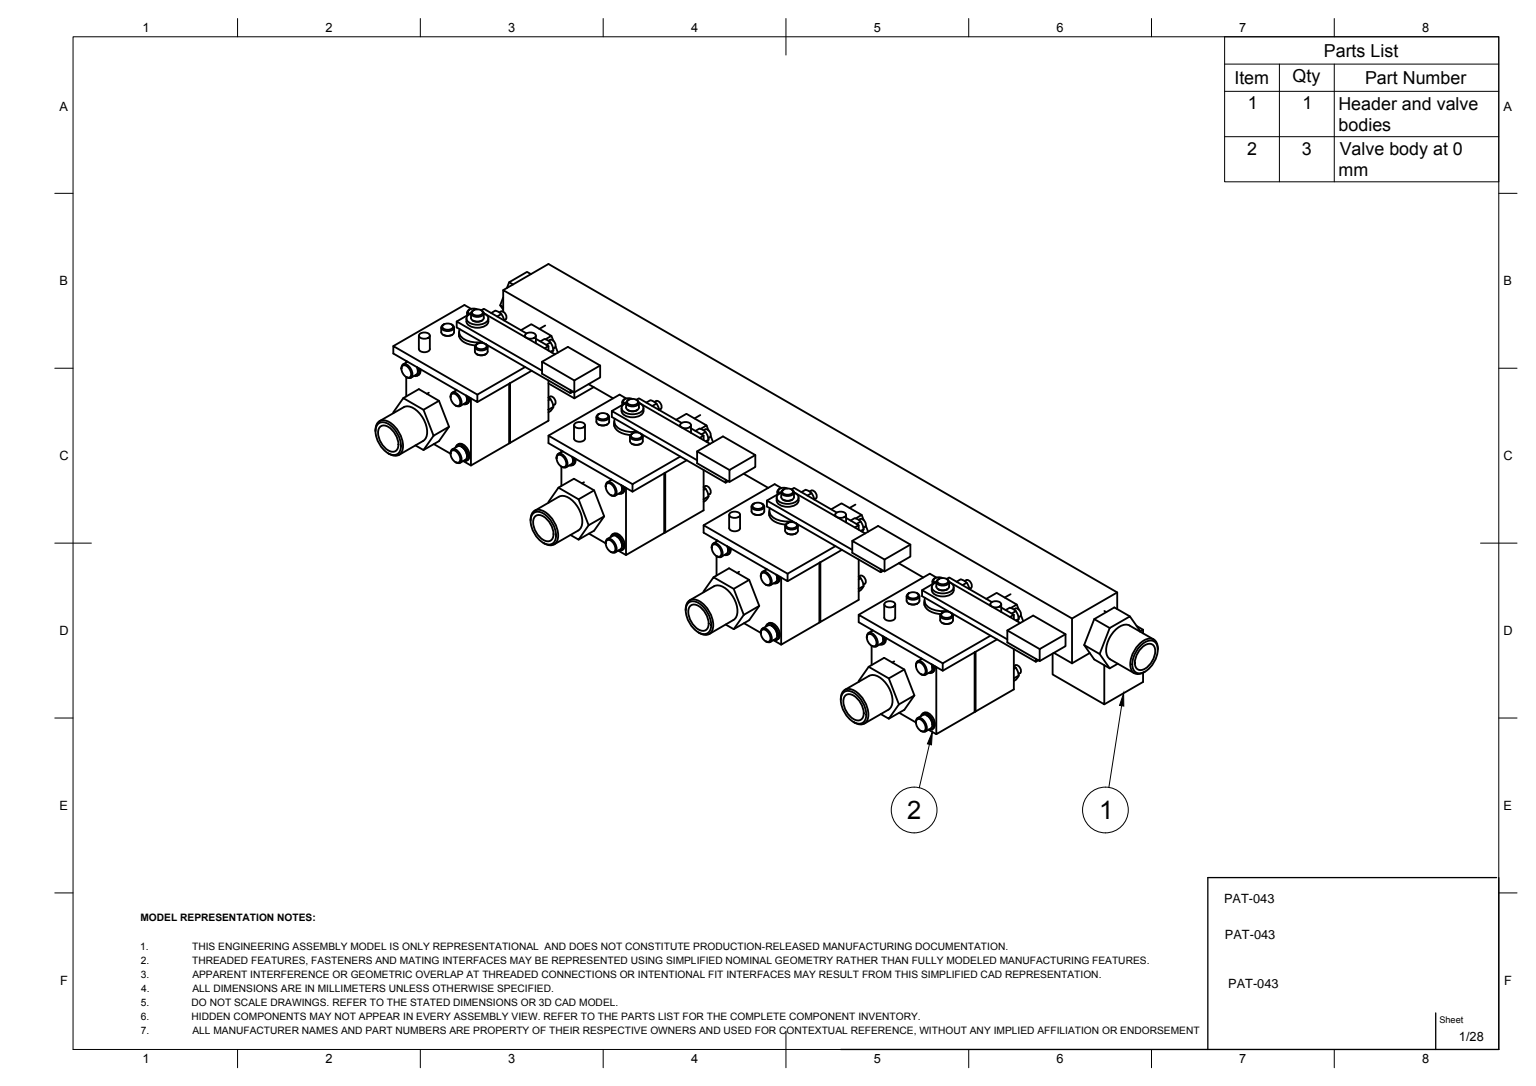
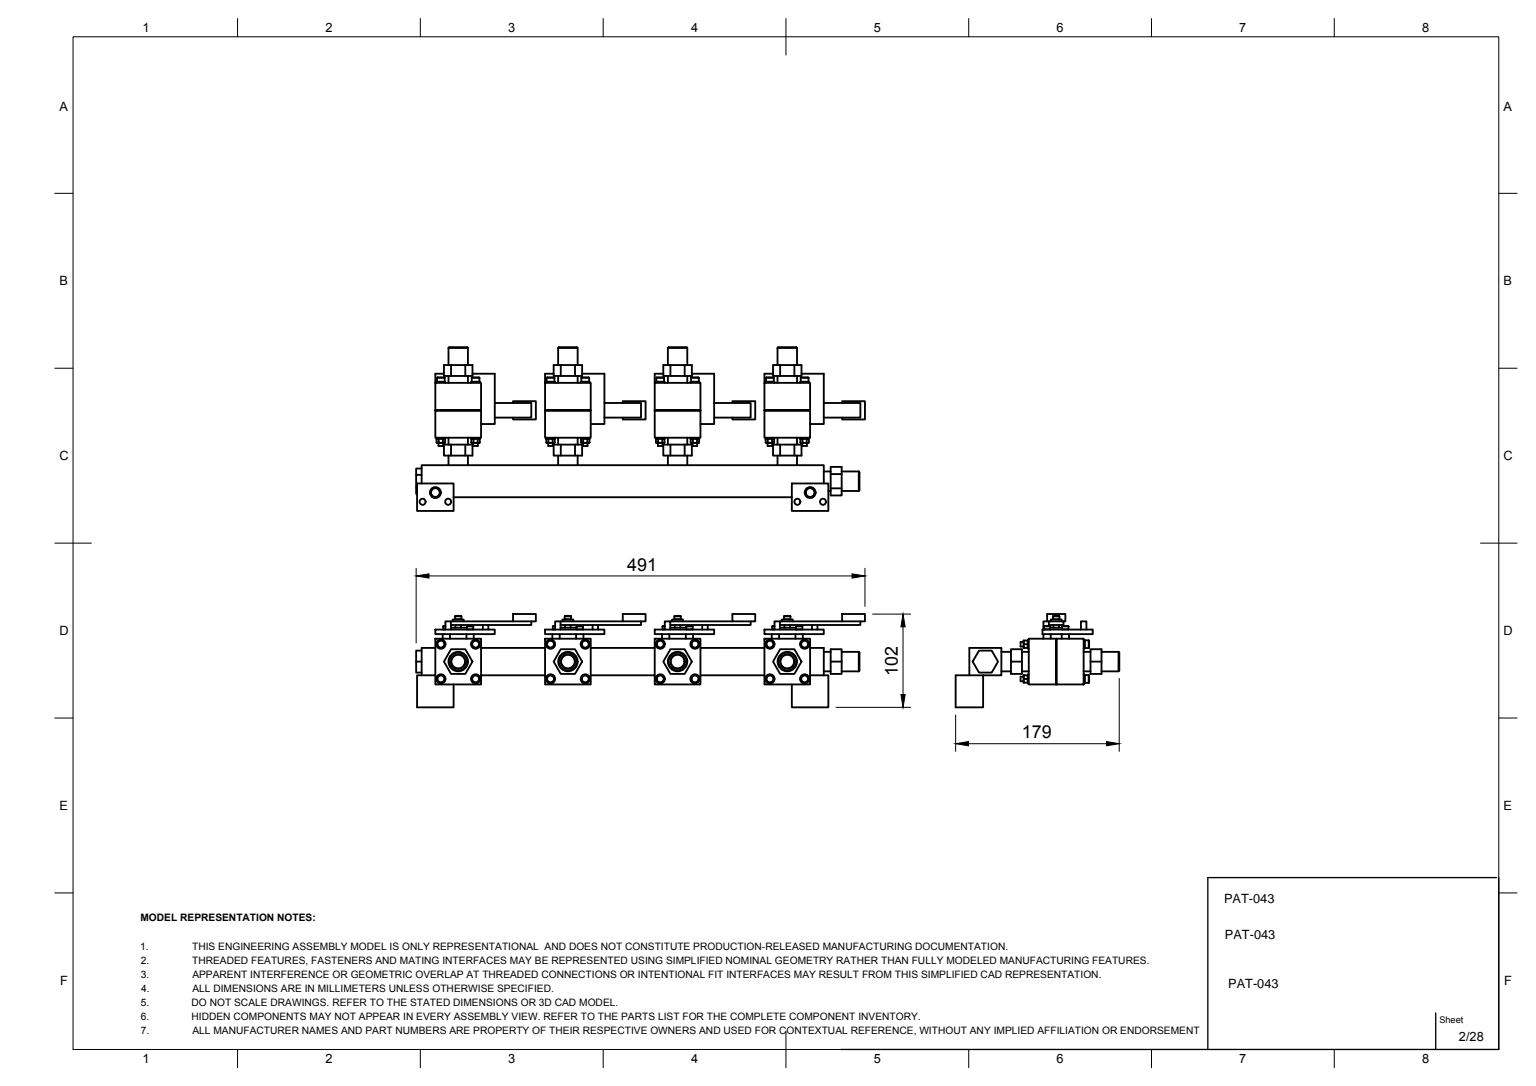
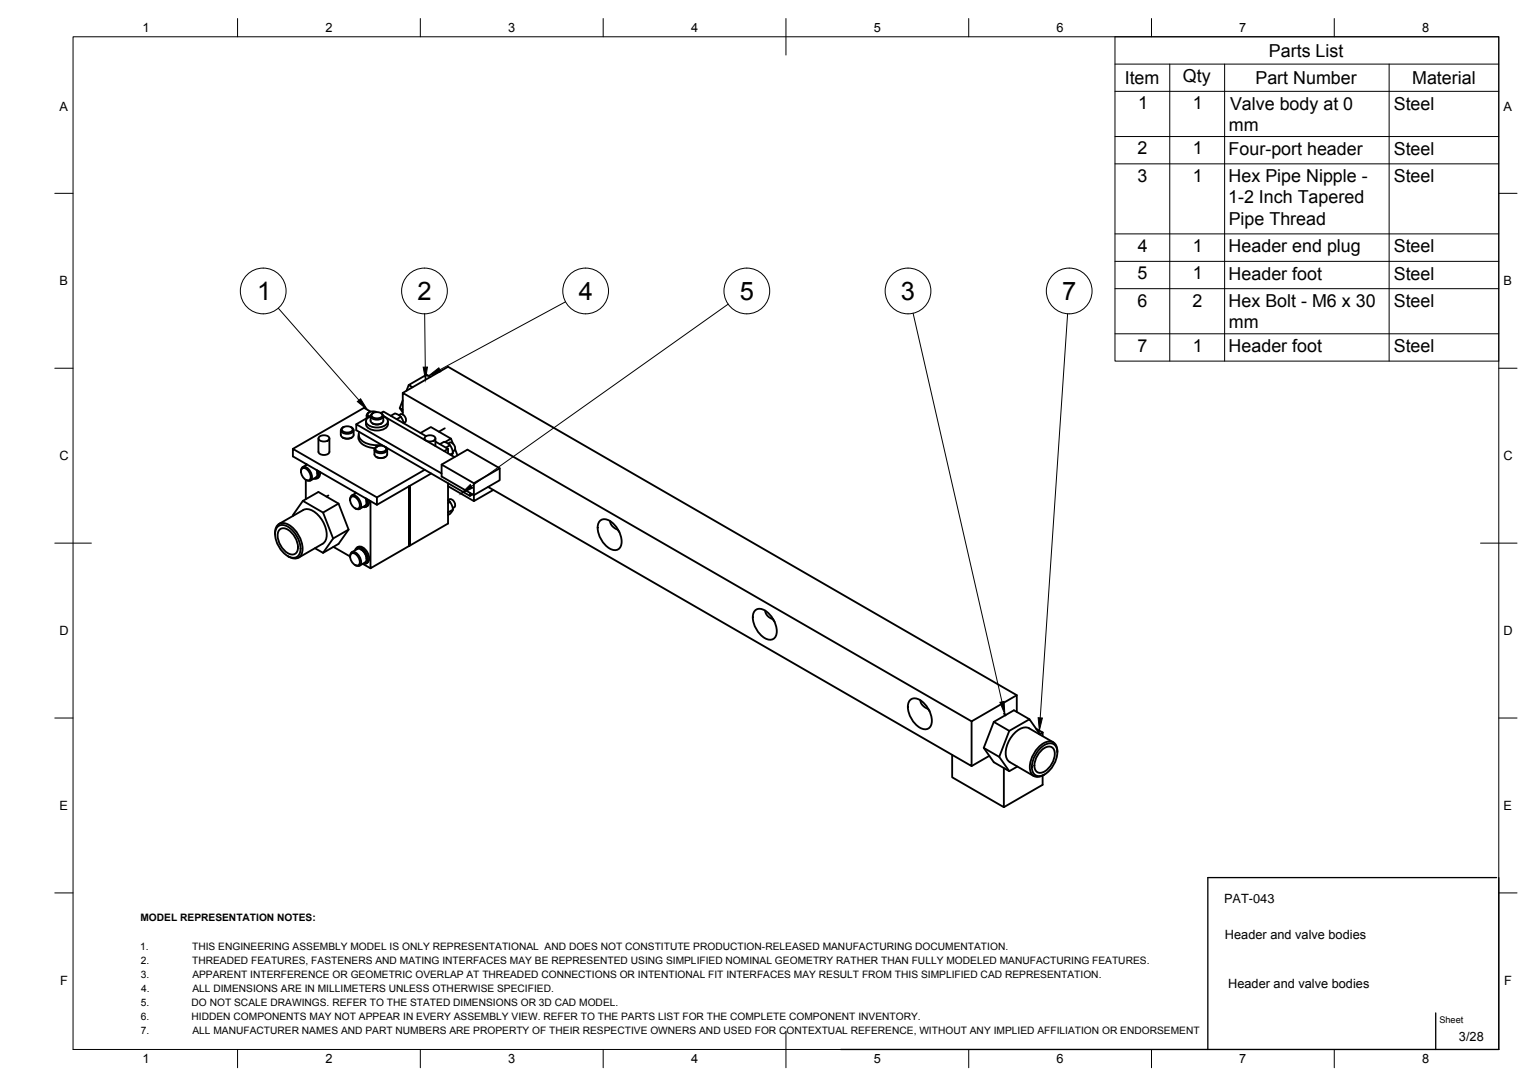
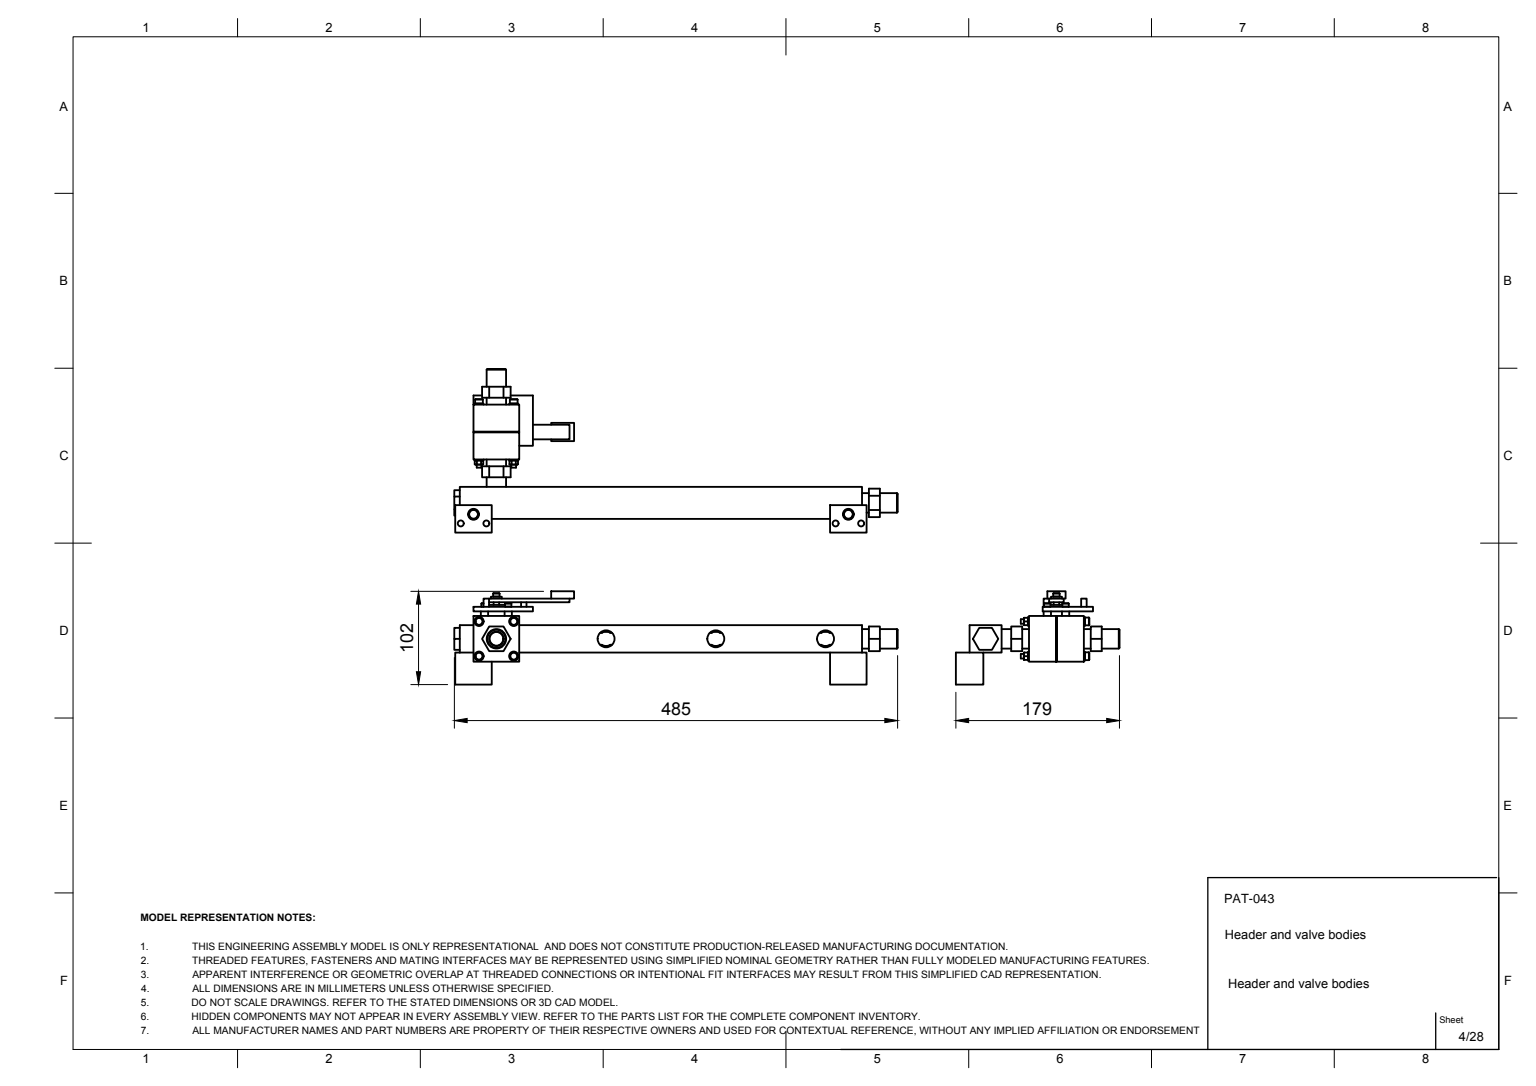
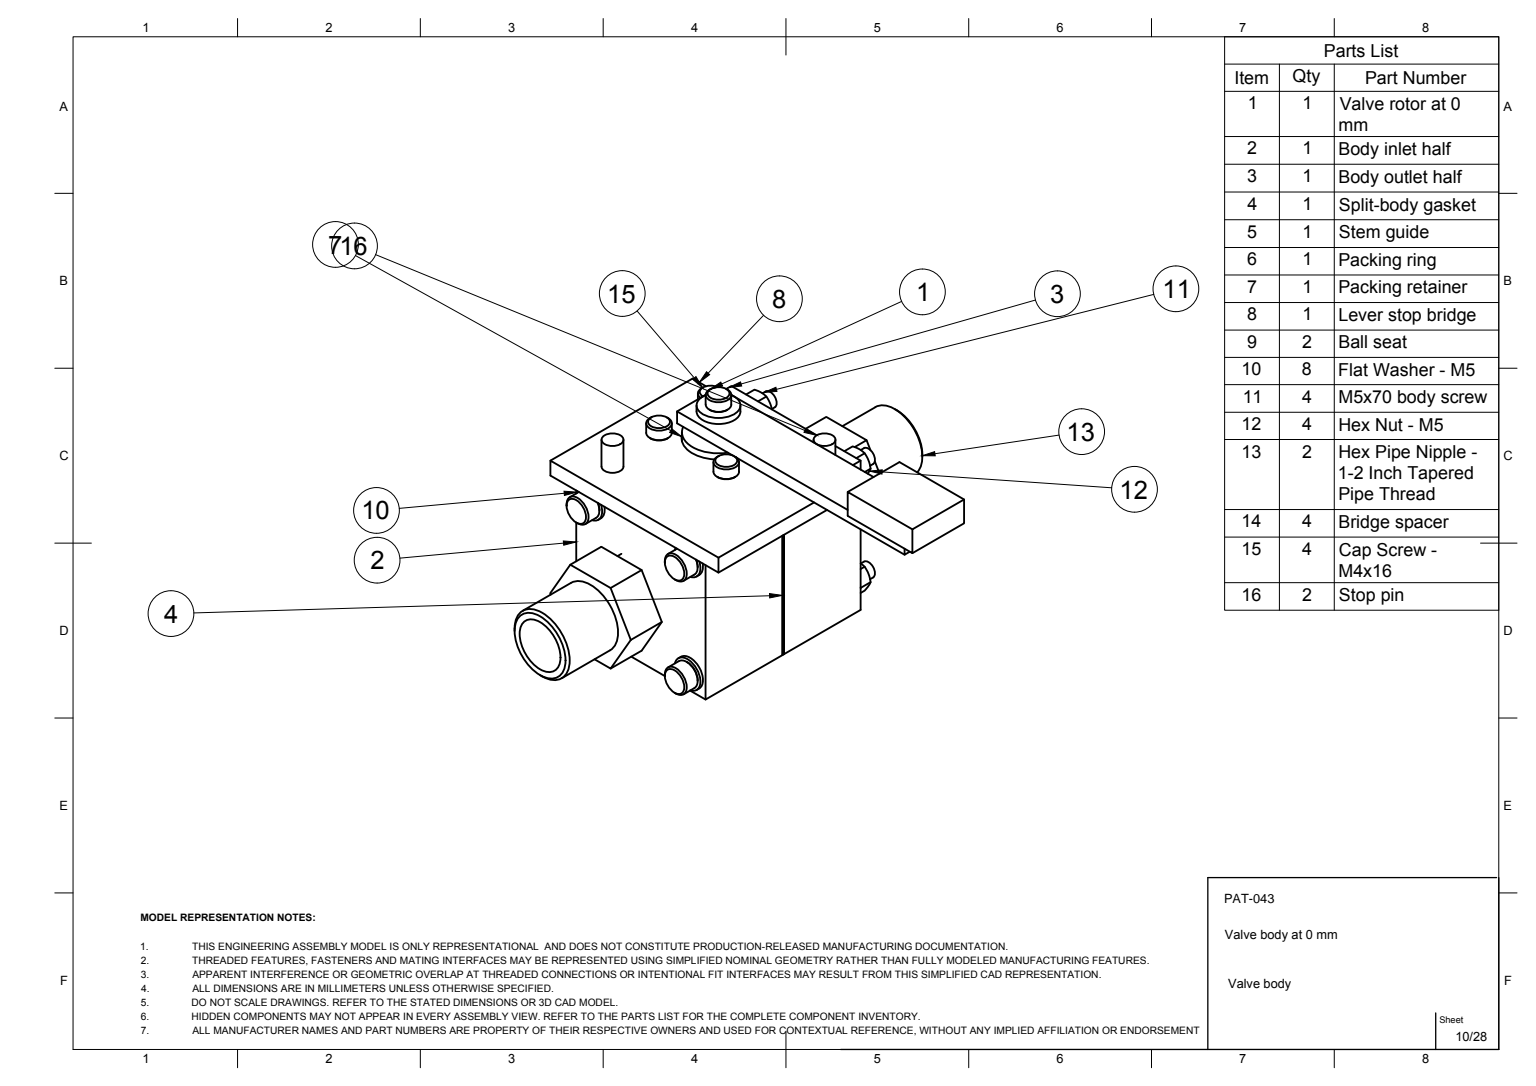
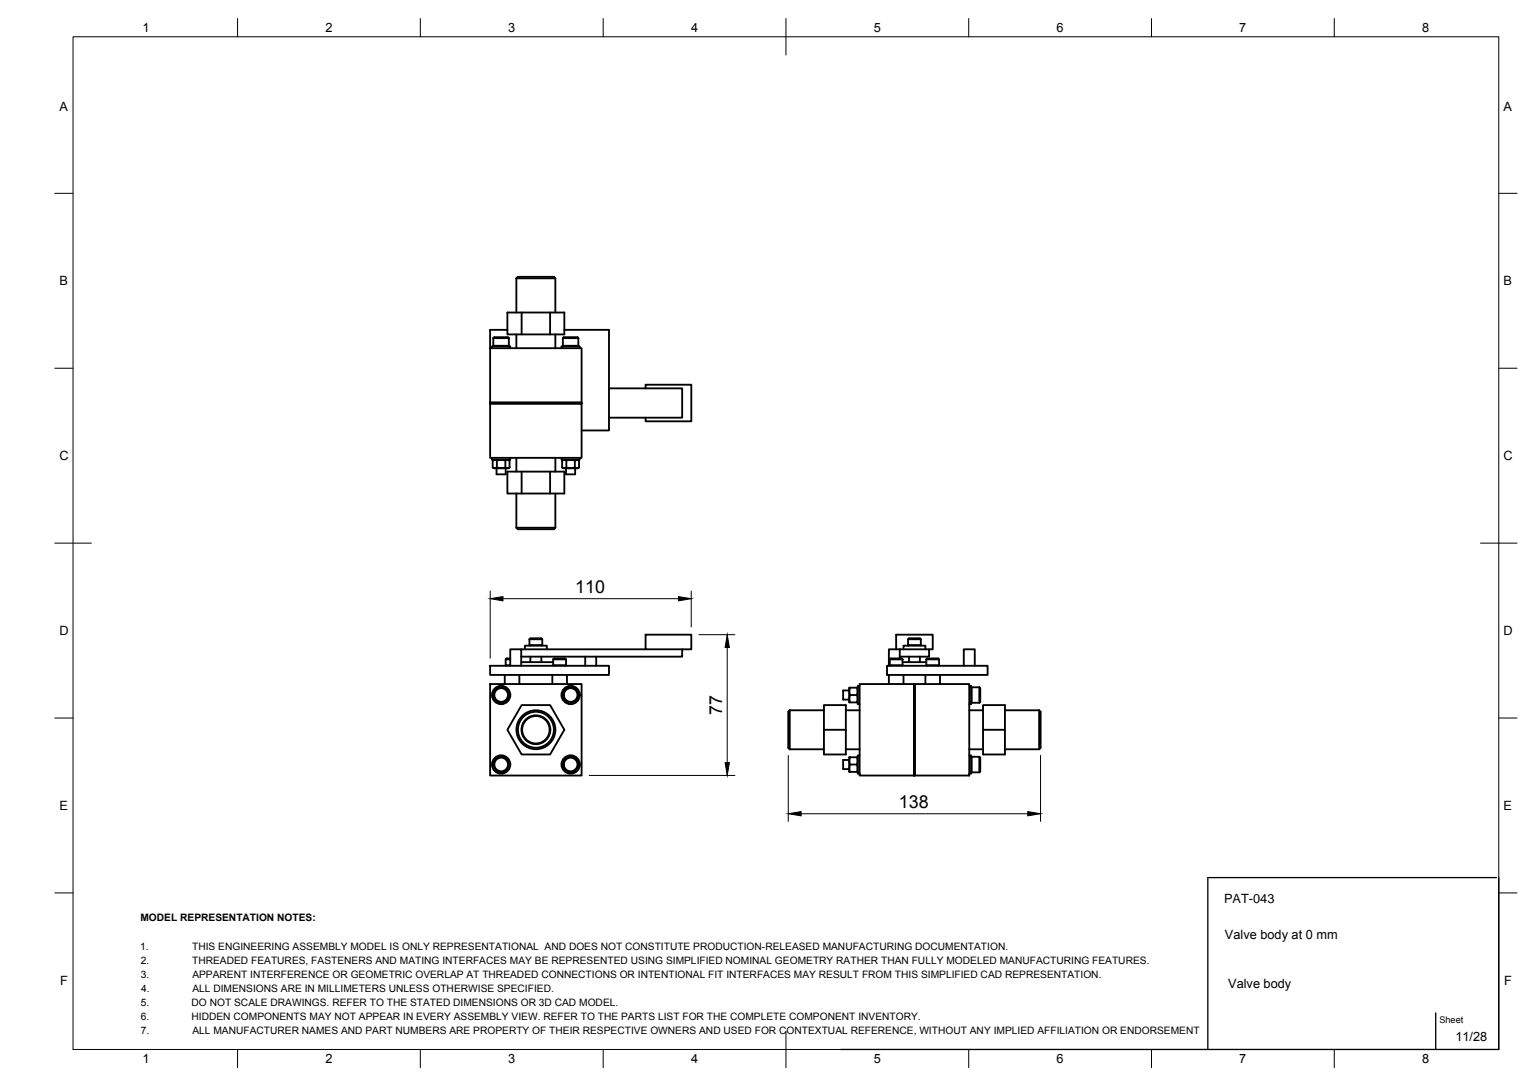
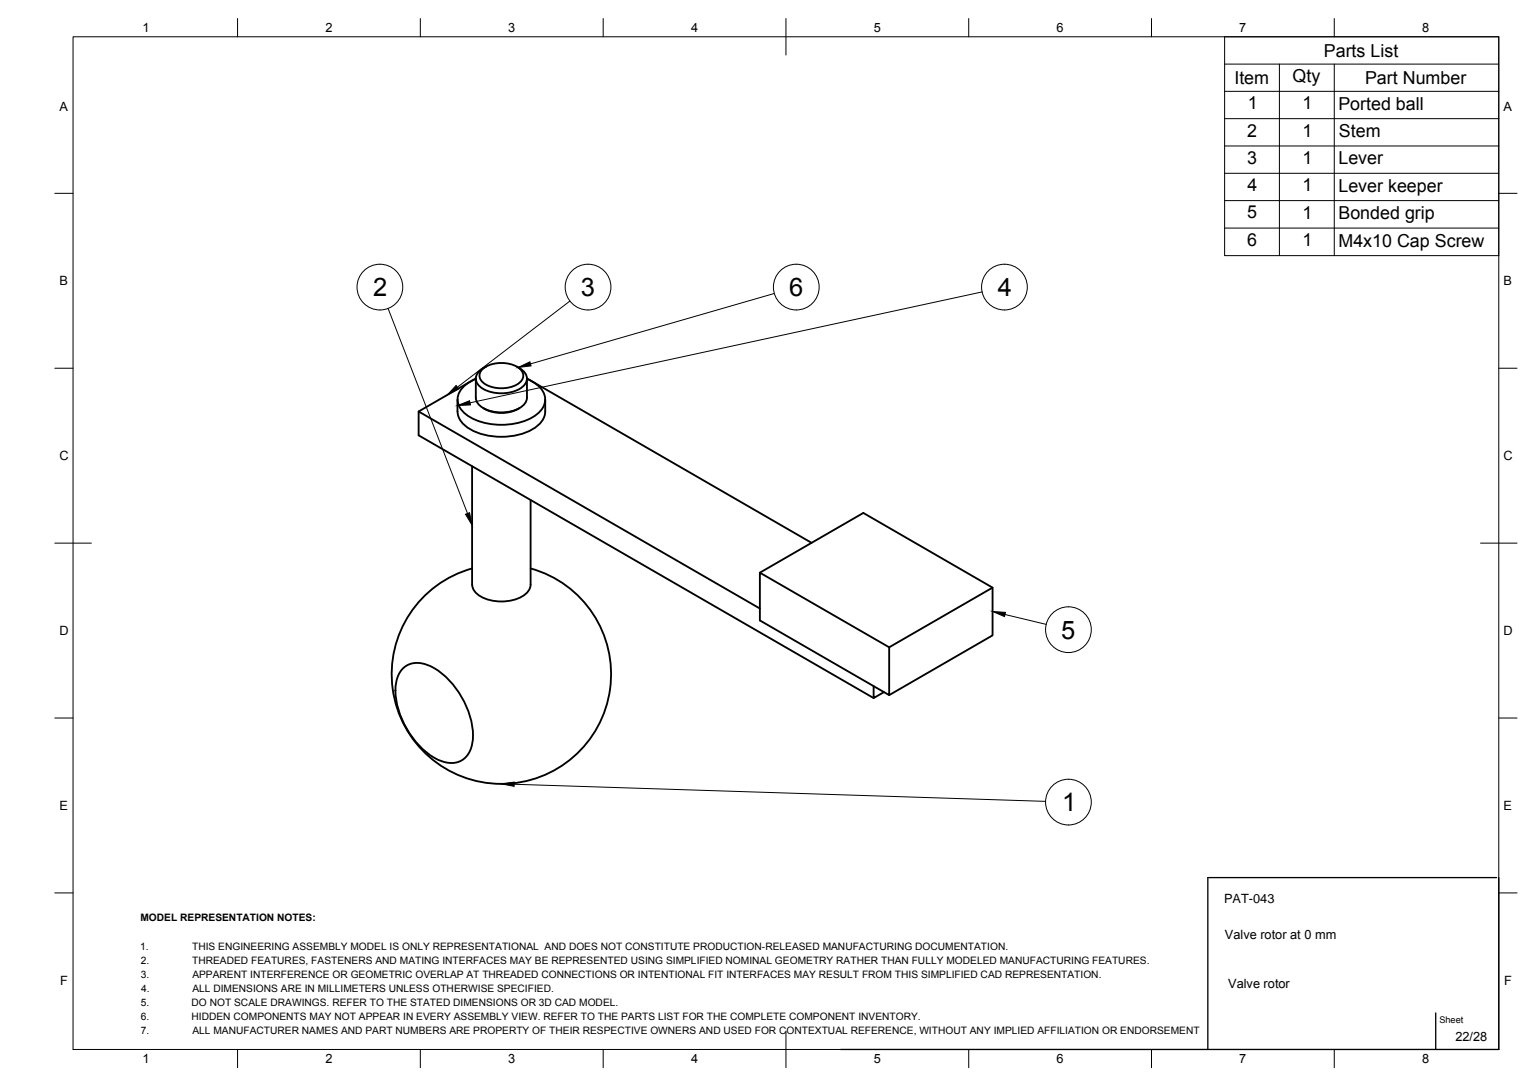
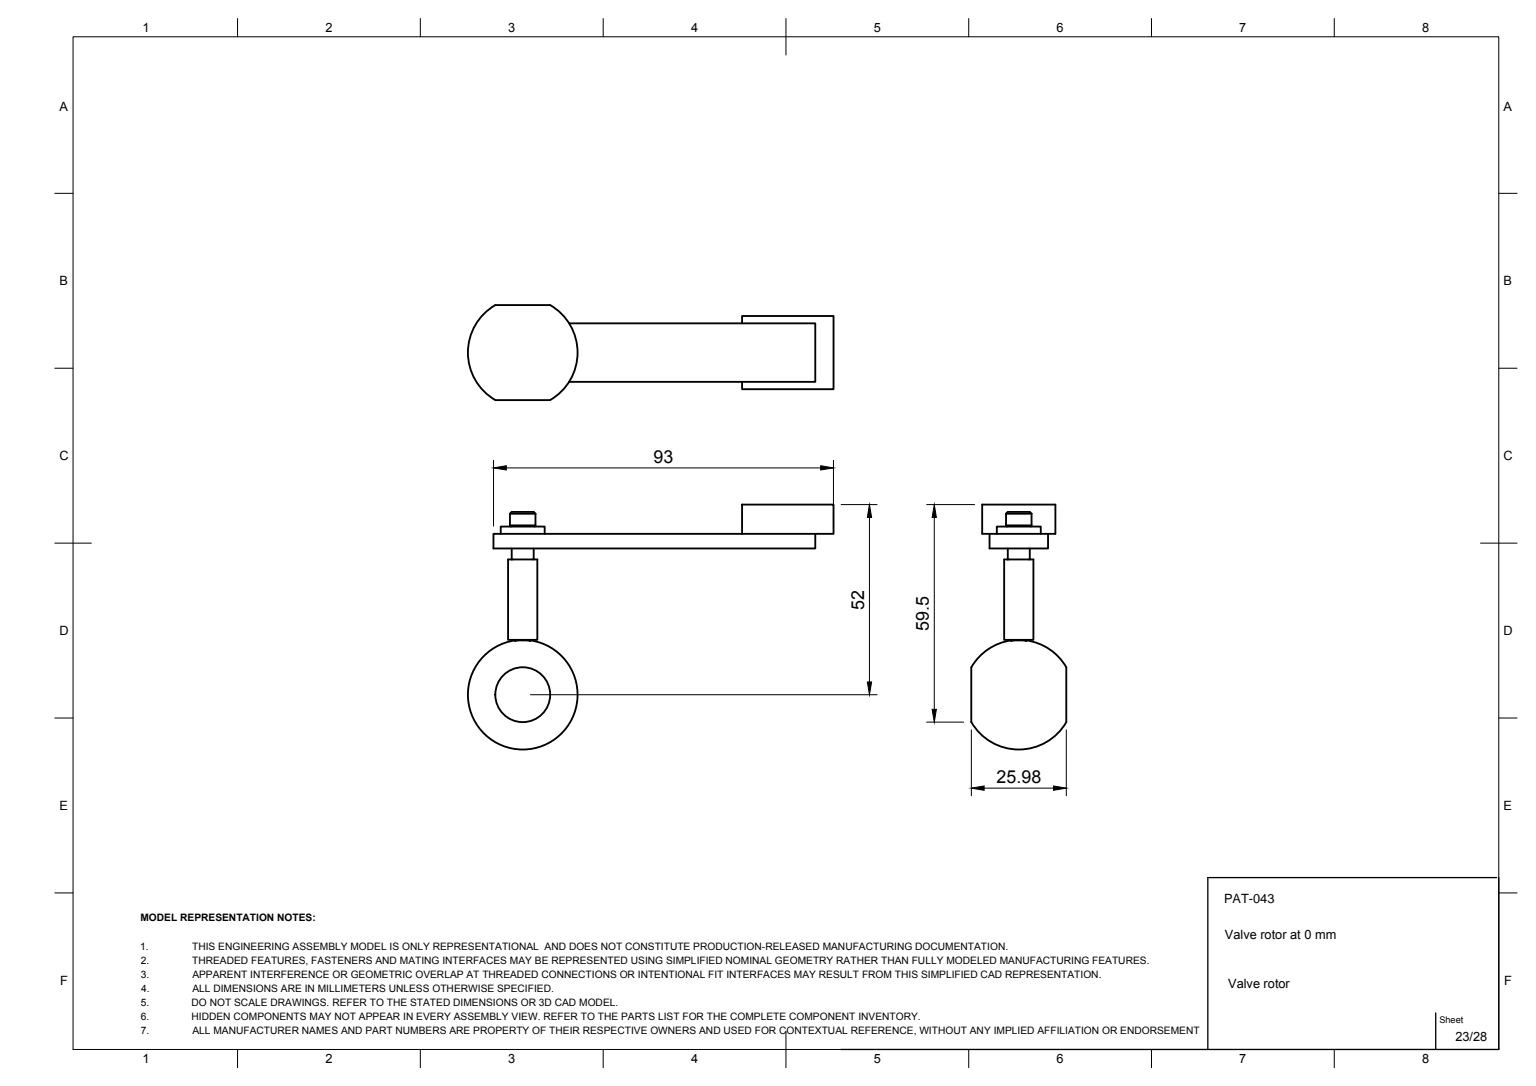
ISO-10303-21;
HEADER;
/* Generated by software containing ST-Developer
 * from STEP Tools, Inc. (www.steptools.com) 
 */

FILE_DESCRIPTION(
/* description */ ('Four-valve pipe header'),
/* implementation_level */ '2;1');

FILE_NAME(
/* name */ 'PAT-043',
/* time_stamp */ '2026-10-29T16:56:19-07:00',
/* author */ (''),
/* organization */ (''),
/* preprocessor_version */ 'ST-DEVELOPER v20.2',
/* originating_system */ 'Autodesk Translation Framework v15.17.0.0',
/* authorisation */ '');

FILE_SCHEMA (('AUTOMOTIVE_DESIGN { 1 0 10303 214 3 1 1 }'));
ENDSEC;

DATA;
#10=MECHANICAL_DESIGN_GEOMETRIC_PRESENTATION_REPRESENTATION('',(#333,#334,
#335,#336,#337,#338,#339,#340,#341,#342,#343,#344,#345,#346,#347,#348,#349,
#350,#351,#352,#353,#354,#355,#356,#357,#358),#10119);
#11=ITEM_DEFINED_TRANSFORMATION($,$,#6411,#6513);
#12=ITEM_DEFINED_TRANSFORMATION($,$,#6427,#6514);
#13=ITEM_DEFINED_TRANSFORMATION($,$,#6462,#6515);
#14=ITEM_DEFINED_TRANSFORMATION($,$,#6473,#6516);
#15=ITEM_DEFINED_TRANSFORMATION($,$,#6482,#6517);
#16=ITEM_DEFINED_TRANSFORMATION($,$,#6489,#6518);
#17=ITEM_DEFINED_TRANSFORMATION($,$,#6106,#6519);
#18=ITEM_DEFINED_TRANSFORMATION($,$,#6149,#6520);
#19=ITEM_DEFINED_TRANSFORMATION($,$,#6192,#6521);
#20=ITEM_DEFINED_TRANSFORMATION($,$,#6219,#6522);
#21=ITEM_DEFINED_TRANSFORMATION($,$,#6232,#6523);
#22=ITEM_DEFINED_TRANSFORMATION($,$,#6236,#6524);
#23=ITEM_DEFINED_TRANSFORMATION($,$,#6249,#6525);
#24=ITEM_DEFINED_TRANSFORMATION($,$,#6279,#6526);
#25=ITEM_DEFINED_TRANSFORMATION($,$,#6279,#6527);
#26=ITEM_DEFINED_TRANSFORMATION($,$,#6318,#6528);
#27=ITEM_DEFINED_TRANSFORMATION($,$,#6290,#6529);
#28=ITEM_DEFINED_TRANSFORMATION($,$,#6318,#6530);
#29=ITEM_DEFINED_TRANSFORMATION($,$,#6329,#6531);
#30=ITEM_DEFINED_TRANSFORMATION($,$,#6318,#6532);
#31=ITEM_DEFINED_TRANSFORMATION($,$,#6290,#6533);
#32=ITEM_DEFINED_TRANSFORMATION($,$,#6318,#6534);
#33=ITEM_DEFINED_TRANSFORMATION($,$,#6329,#6535);
#34=ITEM_DEFINED_TRANSFORMATION($,$,#6318,#6536);
#35=ITEM_DEFINED_TRANSFORMATION($,$,#6290,#6537);
#36=ITEM_DEFINED_TRANSFORMATION($,$,#6318,#6538);
#37=ITEM_DEFINED_TRANSFORMATION($,$,#6329,#6539);
#38=ITEM_DEFINED_TRANSFORMATION($,$,#6318,#6540);
#39=ITEM_DEFINED_TRANSFORMATION($,$,#6290,#6541);
#40=ITEM_DEFINED_TRANSFORMATION($,$,#6318,#6542);
#41=ITEM_DEFINED_TRANSFORMATION($,$,#6329,#6543);
#42=ITEM_DEFINED_TRANSFORMATION($,$,#6345,#6544);
#43=ITEM_DEFINED_TRANSFORMATION($,$,#6345,#6545);
#44=ITEM_DEFINED_TRANSFORMATION($,$,#6369,#6546);
#45=ITEM_DEFINED_TRANSFORMATION($,$,#6378,#6547);
#46=ITEM_DEFINED_TRANSFORMATION($,$,#6369,#6548);
#47=ITEM_DEFINED_TRANSFORMATION($,$,#6378,#6549);
#48=ITEM_DEFINED_TRANSFORMATION($,$,#6369,#6550);
#49=ITEM_DEFINED_TRANSFORMATION($,$,#6378,#6551);
#50=ITEM_DEFINED_TRANSFORMATION($,$,#6369,#6552);
#51=ITEM_DEFINED_TRANSFORMATION($,$,#6378,#6553);
#52=ITEM_DEFINED_TRANSFORMATION($,$,#6404,#6554);
#53=ITEM_DEFINED_TRANSFORMATION($,$,#6404,#6555);
#54=ITEM_DEFINED_TRANSFORMATION($,$,#6410,#6556);
#55=ITEM_DEFINED_TRANSFORMATION($,$,#6105,#6557);
#56=ITEM_DEFINED_TRANSFORMATION($,$,#5897,#6558);
#57=ITEM_DEFINED_TRANSFORMATION($,$,#6019,#6559);
#58=ITEM_DEFINED_TRANSFORMATION($,$,#6032,#6560);
#59=ITEM_DEFINED_TRANSFORMATION($,$,#6060,#6561);
#60=ITEM_DEFINED_TRANSFORMATION($,$,#6345,#6562);
#61=ITEM_DEFINED_TRANSFORMATION($,$,#6088,#6563);
#62=ITEM_DEFINED_TRANSFORMATION($,$,#6088,#6564);
#63=ITEM_DEFINED_TRANSFORMATION($,$,#5896,#6565);
#64=ITEM_DEFINED_TRANSFORMATION($,$,#6105,#6566);
#65=ITEM_DEFINED_TRANSFORMATION($,$,#6105,#6567);
#66=ITEM_DEFINED_TRANSFORMATION($,$,#6105,#6568);
#67=(
REPRESENTATION_RELATIONSHIP($,$,#10264,#10263)
REPRESENTATION_RELATIONSHIP_WITH_TRANSFORMATION(#11)
SHAPE_REPRESENTATION_RELATIONSHIP()
);
#68=(
REPRESENTATION_RELATIONSHIP($,$,#10265,#10263)
REPRESENTATION_RELATIONSHIP_WITH_TRANSFORMATION(#12)
SHAPE_REPRESENTATION_RELATIONSHIP()
);
#69=(
REPRESENTATION_RELATIONSHIP($,$,#10266,#10263)
REPRESENTATION_RELATIONSHIP_WITH_TRANSFORMATION(#13)
SHAPE_REPRESENTATION_RELATIONSHIP()
);
#70=(
REPRESENTATION_RELATIONSHIP($,$,#10267,#10263)
REPRESENTATION_RELATIONSHIP_WITH_TRANSFORMATION(#14)
SHAPE_REPRESENTATION_RELATIONSHIP()
);
#71=(
REPRESENTATION_RELATIONSHIP($,$,#10268,#10263)
REPRESENTATION_RELATIONSHIP_WITH_TRANSFORMATION(#15)
SHAPE_REPRESENTATION_RELATIONSHIP()
);
#72=(
REPRESENTATION_RELATIONSHIP($,$,#10269,#10263)
REPRESENTATION_RELATIONSHIP_WITH_TRANSFORMATION(#16)
SHAPE_REPRESENTATION_RELATIONSHIP()
);
#73=(
REPRESENTATION_RELATIONSHIP($,$,#10248,#10247)
REPRESENTATION_RELATIONSHIP_WITH_TRANSFORMATION(#17)
SHAPE_REPRESENTATION_RELATIONSHIP()
);
#74=(
REPRESENTATION_RELATIONSHIP($,$,#10249,#10247)
REPRESENTATION_RELATIONSHIP_WITH_TRANSFORMATION(#18)
SHAPE_REPRESENTATION_RELATIONSHIP()
);
#75=(
REPRESENTATION_RELATIONSHIP($,$,#10250,#10247)
REPRESENTATION_RELATIONSHIP_WITH_TRANSFORMATION(#19)
SHAPE_REPRESENTATION_RELATIONSHIP()
);
#76=(
REPRESENTATION_RELATIONSHIP($,$,#10251,#10247)
REPRESENTATION_RELATIONSHIP_WITH_TRANSFORMATION(#20)
SHAPE_REPRESENTATION_RELATIONSHIP()
);
#77=(
REPRESENTATION_RELATIONSHIP($,$,#10252,#10247)
REPRESENTATION_RELATIONSHIP_WITH_TRANSFORMATION(#21)
SHAPE_REPRESENTATION_RELATIONSHIP()
);
#78=(
REPRESENTATION_RELATIONSHIP($,$,#10253,#10247)
REPRESENTATION_RELATIONSHIP_WITH_TRANSFORMATION(#22)
SHAPE_REPRESENTATION_RELATIONSHIP()
);
#79=(
REPRESENTATION_RELATIONSHIP($,$,#10254,#10247)
REPRESENTATION_RELATIONSHIP_WITH_TRANSFORMATION(#23)
SHAPE_REPRESENTATION_RELATIONSHIP()
);
#80=(
REPRESENTATION_RELATIONSHIP($,$,#10255,#10247)
REPRESENTATION_RELATIONSHIP_WITH_TRANSFORMATION(#24)
SHAPE_REPRESENTATION_RELATIONSHIP()
);
#81=(
REPRESENTATION_RELATIONSHIP($,$,#10255,#10247)
REPRESENTATION_RELATIONSHIP_WITH_TRANSFORMATION(#25)
SHAPE_REPRESENTATION_RELATIONSHIP()
);
#82=(
REPRESENTATION_RELATIONSHIP($,$,#10257,#10247)
REPRESENTATION_RELATIONSHIP_WITH_TRANSFORMATION(#26)
SHAPE_REPRESENTATION_RELATIONSHIP()
);
#83=(
REPRESENTATION_RELATIONSHIP($,$,#10256,#10247)
REPRESENTATION_RELATIONSHIP_WITH_TRANSFORMATION(#27)
SHAPE_REPRESENTATION_RELATIONSHIP()
);
#84=(
REPRESENTATION_RELATIONSHIP($,$,#10257,#10247)
REPRESENTATION_RELATIONSHIP_WITH_TRANSFORMATION(#28)
SHAPE_REPRESENTATION_RELATIONSHIP()
);
#85=(
REPRESENTATION_RELATIONSHIP($,$,#10258,#10247)
REPRESENTATION_RELATIONSHIP_WITH_TRANSFORMATION(#29)
SHAPE_REPRESENTATION_RELATIONSHIP()
);
#86=(
REPRESENTATION_RELATIONSHIP($,$,#10257,#10247)
REPRESENTATION_RELATIONSHIP_WITH_TRANSFORMATION(#30)
SHAPE_REPRESENTATION_RELATIONSHIP()
);
#87=(
REPRESENTATION_RELATIONSHIP($,$,#10256,#10247)
REPRESENTATION_RELATIONSHIP_WITH_TRANSFORMATION(#31)
SHAPE_REPRESENTATION_RELATIONSHIP()
);
#88=(
REPRESENTATION_RELATIONSHIP($,$,#10257,#10247)
REPRESENTATION_RELATIONSHIP_WITH_TRANSFORMATION(#32)
SHAPE_REPRESENTATION_RELATIONSHIP()
);
#89=(
REPRESENTATION_RELATIONSHIP($,$,#10258,#10247)
REPRESENTATION_RELATIONSHIP_WITH_TRANSFORMATION(#33)
SHAPE_REPRESENTATION_RELATIONSHIP()
);
#90=(
REPRESENTATION_RELATIONSHIP($,$,#10257,#10247)
REPRESENTATION_RELATIONSHIP_WITH_TRANSFORMATION(#34)
SHAPE_REPRESENTATION_RELATIONSHIP()
);
#91=(
REPRESENTATION_RELATIONSHIP($,$,#10256,#10247)
REPRESENTATION_RELATIONSHIP_WITH_TRANSFORMATION(#35)
SHAPE_REPRESENTATION_RELATIONSHIP()
);
#92=(
REPRESENTATION_RELATIONSHIP($,$,#10257,#10247)
REPRESENTATION_RELATIONSHIP_WITH_TRANSFORMATION(#36)
SHAPE_REPRESENTATION_RELATIONSHIP()
);
#93=(
REPRESENTATION_RELATIONSHIP($,$,#10258,#10247)
REPRESENTATION_RELATIONSHIP_WITH_TRANSFORMATION(#37)
SHAPE_REPRESENTATION_RELATIONSHIP()
);
#94=(
REPRESENTATION_RELATIONSHIP($,$,#10257,#10247)
REPRESENTATION_RELATIONSHIP_WITH_TRANSFORMATION(#38)
SHAPE_REPRESENTATION_RELATIONSHIP()
);
#95=(
REPRESENTATION_RELATIONSHIP($,$,#10256,#10247)
REPRESENTATION_RELATIONSHIP_WITH_TRANSFORMATION(#39)
SHAPE_REPRESENTATION_RELATIONSHIP()
);
#96=(
REPRESENTATION_RELATIONSHIP($,$,#10257,#10247)
REPRESENTATION_RELATIONSHIP_WITH_TRANSFORMATION(#40)
SHAPE_REPRESENTATION_RELATIONSHIP()
);
#97=(
REPRESENTATION_RELATIONSHIP($,$,#10258,#10247)
REPRESENTATION_RELATIONSHIP_WITH_TRANSFORMATION(#41)
SHAPE_REPRESENTATION_RELATIONSHIP()
);
#98=(
REPRESENTATION_RELATIONSHIP($,$,#10259,#10247)
REPRESENTATION_RELATIONSHIP_WITH_TRANSFORMATION(#42)
SHAPE_REPRESENTATION_RELATIONSHIP()
);
#99=(
REPRESENTATION_RELATIONSHIP($,$,#10259,#10247)
REPRESENTATION_RELATIONSHIP_WITH_TRANSFORMATION(#43)
SHAPE_REPRESENTATION_RELATIONSHIP()
);
#100=(
REPRESENTATION_RELATIONSHIP($,$,#10260,#10247)
REPRESENTATION_RELATIONSHIP_WITH_TRANSFORMATION(#44)
SHAPE_REPRESENTATION_RELATIONSHIP()
);
#101=(
REPRESENTATION_RELATIONSHIP($,$,#10261,#10247)
REPRESENTATION_RELATIONSHIP_WITH_TRANSFORMATION(#45)
SHAPE_REPRESENTATION_RELATIONSHIP()
);
#102=(
REPRESENTATION_RELATIONSHIP($,$,#10260,#10247)
REPRESENTATION_RELATIONSHIP_WITH_TRANSFORMATION(#46)
SHAPE_REPRESENTATION_RELATIONSHIP()
);
#103=(
REPRESENTATION_RELATIONSHIP($,$,#10261,#10247)
REPRESENTATION_RELATIONSHIP_WITH_TRANSFORMATION(#47)
SHAPE_REPRESENTATION_RELATIONSHIP()
);
#104=(
REPRESENTATION_RELATIONSHIP($,$,#10260,#10247)
REPRESENTATION_RELATIONSHIP_WITH_TRANSFORMATION(#48)
SHAPE_REPRESENTATION_RELATIONSHIP()
);
#105=(
REPRESENTATION_RELATIONSHIP($,$,#10261,#10247)
REPRESENTATION_RELATIONSHIP_WITH_TRANSFORMATION(#49)
SHAPE_REPRESENTATION_RELATIONSHIP()
);
#106=(
REPRESENTATION_RELATIONSHIP($,$,#10260,#10247)
REPRESENTATION_RELATIONSHIP_WITH_TRANSFORMATION(#50)
SHAPE_REPRESENTATION_RELATIONSHIP()
);
#107=(
REPRESENTATION_RELATIONSHIP($,$,#10261,#10247)
REPRESENTATION_RELATIONSHIP_WITH_TRANSFORMATION(#51)
SHAPE_REPRESENTATION_RELATIONSHIP()
);
#108=(
REPRESENTATION_RELATIONSHIP($,$,#10262,#10247)
REPRESENTATION_RELATIONSHIP_WITH_TRANSFORMATION(#52)
SHAPE_REPRESENTATION_RELATIONSHIP()
);
#109=(
REPRESENTATION_RELATIONSHIP($,$,#10262,#10247)
REPRESENTATION_RELATIONSHIP_WITH_TRANSFORMATION(#53)
SHAPE_REPRESENTATION_RELATIONSHIP()
);
#110=(
REPRESENTATION_RELATIONSHIP($,$,#10263,#10247)
REPRESENTATION_RELATIONSHIP_WITH_TRANSFORMATION(#54)
SHAPE_REPRESENTATION_RELATIONSHIP()
);
#111=(
REPRESENTATION_RELATIONSHIP($,$,#10247,#10241)
REPRESENTATION_RELATIONSHIP_WITH_TRANSFORMATION(#55)
SHAPE_REPRESENTATION_RELATIONSHIP()
);
#112=(
REPRESENTATION_RELATIONSHIP($,$,#10242,#10241)
REPRESENTATION_RELATIONSHIP_WITH_TRANSFORMATION(#56)
SHAPE_REPRESENTATION_RELATIONSHIP()
);
#113=(
REPRESENTATION_RELATIONSHIP($,$,#10243,#10241)
REPRESENTATION_RELATIONSHIP_WITH_TRANSFORMATION(#57)
SHAPE_REPRESENTATION_RELATIONSHIP()
);
#114=(
REPRESENTATION_RELATIONSHIP($,$,#10244,#10241)
REPRESENTATION_RELATIONSHIP_WITH_TRANSFORMATION(#58)
SHAPE_REPRESENTATION_RELATIONSHIP()
);
#115=(
REPRESENTATION_RELATIONSHIP($,$,#10245,#10241)
REPRESENTATION_RELATIONSHIP_WITH_TRANSFORMATION(#59)
SHAPE_REPRESENTATION_RELATIONSHIP()
);
#116=(
REPRESENTATION_RELATIONSHIP($,$,#10259,#10241)
REPRESENTATION_RELATIONSHIP_WITH_TRANSFORMATION(#60)
SHAPE_REPRESENTATION_RELATIONSHIP()
);
#117=(
REPRESENTATION_RELATIONSHIP($,$,#10246,#10241)
REPRESENTATION_RELATIONSHIP_WITH_TRANSFORMATION(#61)
SHAPE_REPRESENTATION_RELATIONSHIP()
);
#118=(
REPRESENTATION_RELATIONSHIP($,$,#10246,#10241)
REPRESENTATION_RELATIONSHIP_WITH_TRANSFORMATION(#62)
SHAPE_REPRESENTATION_RELATIONSHIP()
);
#119=(
REPRESENTATION_RELATIONSHIP($,$,#10241,#10240)
REPRESENTATION_RELATIONSHIP_WITH_TRANSFORMATION(#63)
SHAPE_REPRESENTATION_RELATIONSHIP()
);
#120=(
REPRESENTATION_RELATIONSHIP($,$,#10247,#10240)
REPRESENTATION_RELATIONSHIP_WITH_TRANSFORMATION(#64)
SHAPE_REPRESENTATION_RELATIONSHIP()
);
#121=(
REPRESENTATION_RELATIONSHIP($,$,#10247,#10240)
REPRESENTATION_RELATIONSHIP_WITH_TRANSFORMATION(#65)
SHAPE_REPRESENTATION_RELATIONSHIP()
);
#122=(
REPRESENTATION_RELATIONSHIP($,$,#10247,#10240)
REPRESENTATION_RELATIONSHIP_WITH_TRANSFORMATION(#66)
SHAPE_REPRESENTATION_RELATIONSHIP()
);
#123=CONTEXT_DEPENDENT_SHAPE_REPRESENTATION(#67,#10184);
#124=CONTEXT_DEPENDENT_SHAPE_REPRESENTATION(#68,#10185);
#125=CONTEXT_DEPENDENT_SHAPE_REPRESENTATION(#69,#10186);
#126=CONTEXT_DEPENDENT_SHAPE_REPRESENTATION(#70,#10187);
#127=CONTEXT_DEPENDENT_SHAPE_REPRESENTATION(#71,#10188);
#128=CONTEXT_DEPENDENT_SHAPE_REPRESENTATION(#72,#10189);
#129=CONTEXT_DEPENDENT_SHAPE_REPRESENTATION(#73,#10190);
#130=CONTEXT_DEPENDENT_SHAPE_REPRESENTATION(#74,#10191);
#131=CONTEXT_DEPENDENT_SHAPE_REPRESENTATION(#75,#10192);
#132=CONTEXT_DEPENDENT_SHAPE_REPRESENTATION(#76,#10193);
#133=CONTEXT_DEPENDENT_SHAPE_REPRESENTATION(#77,#10194);
#134=CONTEXT_DEPENDENT_SHAPE_REPRESENTATION(#78,#10195);
#135=CONTEXT_DEPENDENT_SHAPE_REPRESENTATION(#79,#10196);
#136=CONTEXT_DEPENDENT_SHAPE_REPRESENTATION(#80,#10197);
#137=CONTEXT_DEPENDENT_SHAPE_REPRESENTATION(#81,#10198);
#138=CONTEXT_DEPENDENT_SHAPE_REPRESENTATION(#82,#10199);
#139=CONTEXT_DEPENDENT_SHAPE_REPRESENTATION(#83,#10200);
#140=CONTEXT_DEPENDENT_SHAPE_REPRESENTATION(#84,#10201);
#141=CONTEXT_DEPENDENT_SHAPE_REPRESENTATION(#85,#10202);
#142=CONTEXT_DEPENDENT_SHAPE_REPRESENTATION(#86,#10203);
#143=CONTEXT_DEPENDENT_SHAPE_REPRESENTATION(#87,#10204);
#144=CONTEXT_DEPENDENT_SHAPE_REPRESENTATION(#88,#10205);
#145=CONTEXT_DEPENDENT_SHAPE_REPRESENTATION(#89,#10206);
#146=CONTEXT_DEPENDENT_SHAPE_REPRESENTATION(#90,#10207);
#147=CONTEXT_DEPENDENT_SHAPE_REPRESENTATION(#91,#10208);
#148=CONTEXT_DEPENDENT_SHAPE_REPRESENTATION(#92,#10209);
#149=CONTEXT_DEPENDENT_SHAPE_REPRESENTATION(#93,#10210);
#150=CONTEXT_DEPENDENT_SHAPE_REPRESENTATION(#94,#10211);
#151=CONTEXT_DEPENDENT_SHAPE_REPRESENTATION(#95,#10212);
#152=CONTEXT_DEPENDENT_SHAPE_REPRESENTATION(#96,#10213);
#153=CONTEXT_DEPENDENT_SHAPE_REPRESENTATION(#97,#10214);
#154=CONTEXT_DEPENDENT_SHAPE_REPRESENTATION(#98,#10215);
#155=CONTEXT_DEPENDENT_SHAPE_REPRESENTATION(#99,#10216);
#156=CONTEXT_DEPENDENT_SHAPE_REPRESENTATION(#100,#10217);
#157=CONTEXT_DEPENDENT_SHAPE_REPRESENTATION(#101,#10218);
#158=CONTEXT_DEPENDENT_SHAPE_REPRESENTATION(#102,#10219);
#159=CONTEXT_DEPENDENT_SHAPE_REPRESENTATION(#103,#10220);
#160=CONTEXT_DEPENDENT_SHAPE_REPRESENTATION(#104,#10221);
#161=CONTEXT_DEPENDENT_SHAPE_REPRESENTATION(#105,#10222);
#162=CONTEXT_DEPENDENT_SHAPE_REPRESENTATION(#106,#10223);
#163=CONTEXT_DEPENDENT_SHAPE_REPRESENTATION(#107,#10224);
#164=CONTEXT_DEPENDENT_SHAPE_REPRESENTATION(#108,#10225);
#165=CONTEXT_DEPENDENT_SHAPE_REPRESENTATION(#109,#10226);
#166=CONTEXT_DEPENDENT_SHAPE_REPRESENTATION(#110,#10227);
#167=CONTEXT_DEPENDENT_SHAPE_REPRESENTATION(#111,#10228);
#168=CONTEXT_DEPENDENT_SHAPE_REPRESENTATION(#112,#10229);
#169=CONTEXT_DEPENDENT_SHAPE_REPRESENTATION(#113,#10230);
#170=CONTEXT_DEPENDENT_SHAPE_REPRESENTATION(#114,#10231);
#171=CONTEXT_DEPENDENT_SHAPE_REPRESENTATION(#115,#10232);
#172=CONTEXT_DEPENDENT_SHAPE_REPRESENTATION(#116,#10233);
#173=CONTEXT_DEPENDENT_SHAPE_REPRESENTATION(#117,#10234);
#174=CONTEXT_DEPENDENT_SHAPE_REPRESENTATION(#118,#10235);
#175=CONTEXT_DEPENDENT_SHAPE_REPRESENTATION(#119,#10236);
#176=CONTEXT_DEPENDENT_SHAPE_REPRESENTATION(#120,#10237);
#177=CONTEXT_DEPENDENT_SHAPE_REPRESENTATION(#121,#10238);
#178=CONTEXT_DEPENDENT_SHAPE_REPRESENTATION(#122,#10239);
#179=NEXT_ASSEMBLY_USAGE_OCCURRENCE('Ported ball:2','Ported ball:2',
'Ported ball:2',#10294,#10295,'Ported ball:2');
#180=NEXT_ASSEMBLY_USAGE_OCCURRENCE('Stem:2','Stem:2','Stem:2',#10294,#10296,
'Stem:2');
#181=NEXT_ASSEMBLY_USAGE_OCCURRENCE('Lever:2','Lever:2','Lever:2',#10294,
#10297,'Lever:2');
#182=NEXT_ASSEMBLY_USAGE_OCCURRENCE('Lever keeper:2','Lever keeper:2',
'Lever keeper:2',#10294,#10298,'Lever keeper:2');
#183=NEXT_ASSEMBLY_USAGE_OCCURRENCE('Bonded grip:2','Bonded grip:2',
'Bonded grip:2',#10294,#10299,'Bonded grip:2');
#184=NEXT_ASSEMBLY_USAGE_OCCURRENCE('M4x10 Cap Screw:2',
'M4x10 Cap Screw:2','M4x10 Cap Screw:2',#10294,#10300,
'M4x10 Cap Screw:2');
#185=NEXT_ASSEMBLY_USAGE_OCCURRENCE('Body inlet half:2',
'Body inlet half:2','Body inlet half:2',#10278,#10279,
'Body inlet half:2');
#186=NEXT_ASSEMBLY_USAGE_OCCURRENCE('Body outlet half:2',
'Body outlet half:2','Body outlet half:2',#10278,#10280,
'Body outlet half:2');
#187=NEXT_ASSEMBLY_USAGE_OCCURRENCE('Split-body gasket:2',
'Split-body gasket:2','Split-body gasket:2',#10278,#10281,
'Split-body gasket:2');
#188=NEXT_ASSEMBLY_USAGE_OCCURRENCE('Stem guide:2','Stem guide:2',
'Stem guide:2',#10278,#10282,'Stem guide:2');
#189=NEXT_ASSEMBLY_USAGE_OCCURRENCE('Packing ring:2','Packing ring:2',
'Packing ring:2',#10278,#10283,'Packing ring:2');
#190=NEXT_ASSEMBLY_USAGE_OCCURRENCE('Packing retainer:2',
'Packing retainer:2','Packing retainer:2',#10278,#10284,
'Packing retainer:2');
#191=NEXT_ASSEMBLY_USAGE_OCCURRENCE('Lever stop bridge:2',
'Lever stop bridge:2','Lever stop bridge:2',#10278,#10285,
'Lever stop bridge:2');
#192=NEXT_ASSEMBLY_USAGE_OCCURRENCE('Ball seat:2','Ball seat:2',
'Ball seat:2',#10278,#10286,'Ball seat:2');
#193=NEXT_ASSEMBLY_USAGE_OCCURRENCE('Ball seat:3','Ball seat:3',
'Ball seat:3',#10278,#10286,'Ball seat:3');
#194=NEXT_ASSEMBLY_USAGE_OCCURRENCE('Flat Washer - M5:2',
'Flat Washer - M5:2','Flat Washer - M5:2',#10278,#10288,
'Flat Washer - M5:2');
#195=NEXT_ASSEMBLY_USAGE_OCCURRENCE('M5x70 body screw:2',
'M5x70 body screw:2','M5x70 body screw:2',#10278,#10287,
'M5x70 body screw:2');
#196=NEXT_ASSEMBLY_USAGE_OCCURRENCE('Flat Washer - M5:3',
'Flat Washer - M5:3','Flat Washer - M5:3',#10278,#10288,
'Flat Washer - M5:3');
#197=NEXT_ASSEMBLY_USAGE_OCCURRENCE('Hex Nut - M5:2','Hex Nut - M5:2',
'Hex Nut - M5:2',#10278,#10289,'Hex Nut - M5:2');
#198=NEXT_ASSEMBLY_USAGE_OCCURRENCE('Flat Washer - M5:4',
'Flat Washer - M5:4','Flat Washer - M5:4',#10278,#10288,
'Flat Washer - M5:4');
#199=NEXT_ASSEMBLY_USAGE_OCCURRENCE('M5x70 body screw:3',
'M5x70 body screw:3','M5x70 body screw:3',#10278,#10287,
'M5x70 body screw:3');
#200=NEXT_ASSEMBLY_USAGE_OCCURRENCE('Flat Washer - M5:5',
'Flat Washer - M5:5','Flat Washer - M5:5',#10278,#10288,
'Flat Washer - M5:5');
#201=NEXT_ASSEMBLY_USAGE_OCCURRENCE('Hex Nut - M5:3','Hex Nut - M5:3',
'Hex Nut - M5:3',#10278,#10289,'Hex Nut - M5:3');
#202=NEXT_ASSEMBLY_USAGE_OCCURRENCE('Flat Washer - M5:6',
'Flat Washer - M5:6','Flat Washer - M5:6',#10278,#10288,
'Flat Washer - M5:6');
#203=NEXT_ASSEMBLY_USAGE_OCCURRENCE('M5x70 body screw:4',
'M5x70 body screw:4','M5x70 body screw:4',#10278,#10287,
'M5x70 body screw:4');
#204=NEXT_ASSEMBLY_USAGE_OCCURRENCE('Flat Washer - M5:7',
'Flat Washer - M5:7','Flat Washer - M5:7',#10278,#10288,
'Flat Washer - M5:7');
#205=NEXT_ASSEMBLY_USAGE_OCCURRENCE('Hex Nut - M5:4','Hex Nut - M5:4',
'Hex Nut - M5:4',#10278,#10289,'Hex Nut - M5:4');
#206=NEXT_ASSEMBLY_USAGE_OCCURRENCE('Flat Washer - M5:8',
'Flat Washer - M5:8','Flat Washer - M5:8',#10278,#10288,
'Flat Washer - M5:8');
#207=NEXT_ASSEMBLY_USAGE_OCCURRENCE('M5x70 body screw:5',
'M5x70 body screw:5','M5x70 body screw:5',#10278,#10287,
'M5x70 body screw:5');
#208=NEXT_ASSEMBLY_USAGE_OCCURRENCE('Flat Washer - M5:9',
'Flat Washer - M5:9','Flat Washer - M5:9',#10278,#10288,
'Flat Washer - M5:9');
#209=NEXT_ASSEMBLY_USAGE_OCCURRENCE('Hex Nut - M5:5','Hex Nut - M5:5',
'Hex Nut - M5:5',#10278,#10289,'Hex Nut - M5:5');
#210=NEXT_ASSEMBLY_USAGE_OCCURRENCE(
'Hex Pipe Nipple - 1-2 Inch Tapered Pipe Thread:2',
'Hex Pipe Nipple - 1-2 Inch Tapered Pipe Thread:2',
'Hex Pipe Nipple - 1-2 Inch Tapered Pipe Thread:2',#10278,#10290,
'Hex Pipe Nipple - 1-2 Inch Tapered Pipe Thread:2');
#211=NEXT_ASSEMBLY_USAGE_OCCURRENCE(
'Hex Pipe Nipple - 1-2 Inch Tapered Pipe Thread:3',
'Hex Pipe Nipple - 1-2 Inch Tapered Pipe Thread:3',
'Hex Pipe Nipple - 1-2 Inch Tapered Pipe Thread:3',#10278,#10290,
'Hex Pipe Nipple - 1-2 Inch Tapered Pipe Thread:3');
#212=NEXT_ASSEMBLY_USAGE_OCCURRENCE('Bridge spacer:2','Bridge spacer:2',
'Bridge spacer:2',#10278,#10291,'Bridge spacer:2');
#213=NEXT_ASSEMBLY_USAGE_OCCURRENCE('Cap Screw - M4x16:2',
'Cap Screw - M4x16:2','Cap Screw - M4x16:2',#10278,#10292,
'Cap Screw - M4x16:2');
#214=NEXT_ASSEMBLY_USAGE_OCCURRENCE('Bridge spacer:3','Bridge spacer:3',
'Bridge spacer:3',#10278,#10291,'Bridge spacer:3');
#215=NEXT_ASSEMBLY_USAGE_OCCURRENCE('Cap Screw - M4x16:3',
'Cap Screw - M4x16:3','Cap Screw - M4x16:3',#10278,#10292,
'Cap Screw - M4x16:3');
#216=NEXT_ASSEMBLY_USAGE_OCCURRENCE('Bridge spacer:4','Bridge spacer:4',
'Bridge spacer:4',#10278,#10291,'Bridge spacer:4');
#217=NEXT_ASSEMBLY_USAGE_OCCURRENCE('Cap Screw - M4x16:4',
'Cap Screw - M4x16:4','Cap Screw - M4x16:4',#10278,#10292,
'Cap Screw - M4x16:4');
#218=NEXT_ASSEMBLY_USAGE_OCCURRENCE('Bridge spacer:5','Bridge spacer:5',
'Bridge spacer:5',#10278,#10291,'Bridge spacer:5');
#219=NEXT_ASSEMBLY_USAGE_OCCURRENCE('Cap Screw - M4x16:5',
'Cap Screw - M4x16:5','Cap Screw - M4x16:5',#10278,#10292,
'Cap Screw - M4x16:5');
#220=NEXT_ASSEMBLY_USAGE_OCCURRENCE('Stop pin:2','Stop pin:2',
'Stop pin:2',#10278,#10293,'Stop pin:2');
#221=NEXT_ASSEMBLY_USAGE_OCCURRENCE('Stop pin:3','Stop pin:3',
'Stop pin:3',#10278,#10293,'Stop pin:3');
#222=NEXT_ASSEMBLY_USAGE_OCCURRENCE('Valve rotor:1','Valve rotor:1',
'Valve rotor:1',#10278,#10294,'Valve rotor:1');
#223=NEXT_ASSEMBLY_USAGE_OCCURRENCE('Valve body:1','Valve body:1',
'Valve body:1',#10272,#10278,'Valve body:1');
#224=NEXT_ASSEMBLY_USAGE_OCCURRENCE('Four-port header:1',
'Four-port header:1','Four-port header:1',#10272,#10273,
'Four-port header:1');
#225=NEXT_ASSEMBLY_USAGE_OCCURRENCE('Header end plug:1',
'Header end plug:1','Header end plug:1',#10272,#10274,
'Header end plug:1');
#226=NEXT_ASSEMBLY_USAGE_OCCURRENCE('Header foot:1','Header foot:1',
'Header foot:1',#10272,#10275,'Header foot:1');
#227=NEXT_ASSEMBLY_USAGE_OCCURRENCE('Header foot (1):1',
'Header foot (1):1','Header foot (1):1',#10272,#10276,
'Header foot (1):1');
#228=NEXT_ASSEMBLY_USAGE_OCCURRENCE(
'Hex Pipe Nipple - 1-2 Inch Tapered Pipe Thread:10',
'Hex Pipe Nipple - 1-2 Inch Tapered Pipe Thread:10',
'Hex Pipe Nipple - 1-2 Inch Tapered Pipe Thread:10',#10272,#10290,
'Hex Pipe Nipple - 1-2 Inch Tapered Pipe Thread:10');
#229=NEXT_ASSEMBLY_USAGE_OCCURRENCE('Hex Bolt - M6 x 30 mm:2',
'Hex Bolt - M6 x 30 mm:2','Hex Bolt - M6 x 30 mm:2',#10272,#10277,
'Hex Bolt - M6 x 30 mm:2');
#230=NEXT_ASSEMBLY_USAGE_OCCURRENCE('Hex Bolt - M6 x 30 mm:3',
'Hex Bolt - M6 x 30 mm:3','Hex Bolt - M6 x 30 mm:3',#10272,#10277,
'Hex Bolt - M6 x 30 mm:3');
#231=NEXT_ASSEMBLY_USAGE_OCCURRENCE('Header and valve bodies:1',
'Header and valve bodies:1','Header and valve bodies:1',#10271,#10272,
'Header and valve bodies:1');
#232=NEXT_ASSEMBLY_USAGE_OCCURRENCE('Valve body:2','Valve body:2',
'Valve body:2',#10271,#10278,'Valve body:2');
#233=NEXT_ASSEMBLY_USAGE_OCCURRENCE('Valve body:3','Valve body:3',
'Valve body:3',#10271,#10278,'Valve body:3');
#234=NEXT_ASSEMBLY_USAGE_OCCURRENCE('Valve body:4','Valve body:4',
'Valve body:4',#10271,#10278,'Valve body:4');
#235=ORIENTED_CLOSED_SHELL('',*,#5592,.F.);
#236=ORIENTED_CLOSED_SHELL('',*,#5599,.F.);
#237=ORIENTED_CLOSED_SHELL('',*,#5606,.F.);
#238=BREP_WITH_VOIDS('Body1',#5593,(#235));
#239=BREP_WITH_VOIDS('Body1',#5598,(#236));
#240=BREP_WITH_VOIDS('Body1',#5607,(#237));
#241=TOROIDAL_SURFACE('',#6233,0.5,0.1);
#242=SPHERICAL_SURFACE('',#6142,1.6);
#243=SPHERICAL_SURFACE('',#6185,1.6);
#244=SPHERICAL_SURFACE('',#6280,1.5);
#245=SPHERICAL_SURFACE('',#6425,1.5);
#246=(
BOUNDED_CURVE()
B_SPLINE_CURVE(2,(#8906,#8907,#8908),.UNSPECIFIED.,.F.,.F.)
B_SPLINE_CURVE_WITH_KNOTS((3,3),(0.144988513094728,0.791574906712449),
 .UNSPECIFIED.)
CURVE()
GEOMETRIC_REPRESENTATION_ITEM()
RATIONAL_B_SPLINE_CURVE((1.09282032302755,1.26188021535082,1.09282032302931))
REPRESENTATION_ITEM('')
);
#247=(
BOUNDED_CURVE()
B_SPLINE_CURVE(2,(#8910,#8911,#8912),.UNSPECIFIED.,.F.,.F.)
B_SPLINE_CURVE_WITH_KNOTS((3,3),(0.144988513094728,0.791574906712449),
 .UNSPECIFIED.)
CURVE()
GEOMETRIC_REPRESENTATION_ITEM()
RATIONAL_B_SPLINE_CURVE((1.09282032302755,1.26188021535082,1.09282032302931))
REPRESENTATION_ITEM('')
);
#248=(
BOUNDED_CURVE()
B_SPLINE_CURVE(2,(#8914,#8915,#8916),.UNSPECIFIED.,.F.,.F.)
B_SPLINE_CURVE_WITH_KNOTS((3,3),(0.144988513094728,0.791574906712449),
 .UNSPECIFIED.)
CURVE()
GEOMETRIC_REPRESENTATION_ITEM()
RATIONAL_B_SPLINE_CURVE((1.09282032302755,1.26188021535082,1.09282032302931))
REPRESENTATION_ITEM('')
);
#249=(
BOUNDED_CURVE()
B_SPLINE_CURVE(2,(#8918,#8919,#8920),.UNSPECIFIED.,.F.,.F.)
B_SPLINE_CURVE_WITH_KNOTS((3,3),(0.144988513094728,0.791574906712449),
 .UNSPECIFIED.)
CURVE()
GEOMETRIC_REPRESENTATION_ITEM()
RATIONAL_B_SPLINE_CURVE((1.09282032302755,1.26188021535082,1.09282032302931))
REPRESENTATION_ITEM('')
);
#250=(
BOUNDED_CURVE()
B_SPLINE_CURVE(2,(#8922,#8923,#8924),.UNSPECIFIED.,.F.,.F.)
B_SPLINE_CURVE_WITH_KNOTS((3,3),(0.144988513094728,0.791574906712449),
 .UNSPECIFIED.)
CURVE()
GEOMETRIC_REPRESENTATION_ITEM()
RATIONAL_B_SPLINE_CURVE((1.09282032302755,1.26188021535082,1.09282032302931))
REPRESENTATION_ITEM('')
);
#251=(
BOUNDED_CURVE()
B_SPLINE_CURVE(2,(#8925,#8926,#8927),.UNSPECIFIED.,.F.,.F.)
B_SPLINE_CURVE_WITH_KNOTS((3,3),(0.144988513094727,0.791574906712449),
 .UNSPECIFIED.)
CURVE()
GEOMETRIC_REPRESENTATION_ITEM()
RATIONAL_B_SPLINE_CURVE((1.09282032302755,1.26188021535082,1.09282032302931))
REPRESENTATION_ITEM('')
);
#252=(
BOUNDED_CURVE()
B_SPLINE_CURVE(2,(#9474,#9475,#9476),.UNSPECIFIED.,.F.,.F.)
B_SPLINE_CURVE_WITH_KNOTS((3,3),(0.140651836354967,0.670383167684795),
 .UNSPECIFIED.)
CURVE()
GEOMETRIC_REPRESENTATION_ITEM()
RATIONAL_B_SPLINE_CURVE((1.11602540378444,1.28867513459481,1.11602540378444))
REPRESENTATION_ITEM('')
);
#253=(
BOUNDED_CURVE()
B_SPLINE_CURVE(2,(#9478,#9479,#9480),.UNSPECIFIED.,.F.,.F.)
B_SPLINE_CURVE_WITH_KNOTS((3,3),(0.140651836354967,0.670383167684795),
 .UNSPECIFIED.)
CURVE()
GEOMETRIC_REPRESENTATION_ITEM()
RATIONAL_B_SPLINE_CURVE((1.11602540378444,1.28867513459481,1.11602540378444))
REPRESENTATION_ITEM('')
);
#254=(
BOUNDED_CURVE()
B_SPLINE_CURVE(2,(#9485,#9486,#9487),.UNSPECIFIED.,.F.,.F.)
B_SPLINE_CURVE_WITH_KNOTS((3,3),(0.140651836354967,0.670383167684795),
 .UNSPECIFIED.)
CURVE()
GEOMETRIC_REPRESENTATION_ITEM()
RATIONAL_B_SPLINE_CURVE((1.11602540378444,1.28867513459481,1.11602540378444))
REPRESENTATION_ITEM('')
);
#255=(
BOUNDED_CURVE()
B_SPLINE_CURVE(2,(#9489,#9490,#9491),.UNSPECIFIED.,.F.,.F.)
B_SPLINE_CURVE_WITH_KNOTS((3,3),(0.140651836354967,0.670383167684795),
 .UNSPECIFIED.)
CURVE()
GEOMETRIC_REPRESENTATION_ITEM()
RATIONAL_B_SPLINE_CURVE((1.11602540378444,1.28867513459481,1.11602540378444))
REPRESENTATION_ITEM('')
);
#256=(
BOUNDED_CURVE()
B_SPLINE_CURVE(2,(#9493,#9494,#9495),.UNSPECIFIED.,.F.,.F.)
B_SPLINE_CURVE_WITH_KNOTS((3,3),(0.140651836354967,0.670383167684795),
 .UNSPECIFIED.)
CURVE()
GEOMETRIC_REPRESENTATION_ITEM()
RATIONAL_B_SPLINE_CURVE((1.11602540378444,1.28867513459481,1.11602540378444))
REPRESENTATION_ITEM('')
);
#257=(
BOUNDED_CURVE()
B_SPLINE_CURVE(2,(#9496,#9497,#9498),.UNSPECIFIED.,.F.,.F.)
B_SPLINE_CURVE_WITH_KNOTS((3,3),(0.140651836354967,0.670383167684795),
 .UNSPECIFIED.)
CURVE()
GEOMETRIC_REPRESENTATION_ITEM()
RATIONAL_B_SPLINE_CURVE((1.11602540378444,1.28867513459481,1.11602540378444))
REPRESENTATION_ITEM('')
);
#258=(
BOUNDED_CURVE()
B_SPLINE_CURVE(2,(#9505,#9506,#9507),.UNSPECIFIED.,.F.,.F.)
B_SPLINE_CURVE_WITH_KNOTS((3,3),(0.140651836354967,0.670383167684795),
 .UNSPECIFIED.)
CURVE()
GEOMETRIC_REPRESENTATION_ITEM()
RATIONAL_B_SPLINE_CURVE((1.11602540378444,1.28867513459481,1.11602540378444))
REPRESENTATION_ITEM('')
);
#259=(
BOUNDED_CURVE()
B_SPLINE_CURVE(2,(#9509,#9510,#9511),.UNSPECIFIED.,.F.,.F.)
B_SPLINE_CURVE_WITH_KNOTS((3,3),(0.140651836354967,0.670383167684796),
 .UNSPECIFIED.)
CURVE()
GEOMETRIC_REPRESENTATION_ITEM()
RATIONAL_B_SPLINE_CURVE((1.11602540378444,1.28867513459481,1.11602540378444))
REPRESENTATION_ITEM('')
);
#260=(
BOUNDED_CURVE()
B_SPLINE_CURVE(2,(#9513,#9514,#9515),.UNSPECIFIED.,.F.,.F.)
B_SPLINE_CURVE_WITH_KNOTS((3,3),(0.140651836354967,0.670383167684795),
 .UNSPECIFIED.)
CURVE()
GEOMETRIC_REPRESENTATION_ITEM()
RATIONAL_B_SPLINE_CURVE((1.11602540378444,1.28867513459481,1.11602540378444))
REPRESENTATION_ITEM('')
);
#261=(
BOUNDED_CURVE()
B_SPLINE_CURVE(2,(#9517,#9518,#9519),.UNSPECIFIED.,.F.,.F.)
B_SPLINE_CURVE_WITH_KNOTS((3,3),(0.140651836354967,0.670383167684795),
 .UNSPECIFIED.)
CURVE()
GEOMETRIC_REPRESENTATION_ITEM()
RATIONAL_B_SPLINE_CURVE((1.11602540378444,1.28867513459482,1.11602540378444))
REPRESENTATION_ITEM('')
);
#262=(
BOUNDED_CURVE()
B_SPLINE_CURVE(2,(#9521,#9522,#9523),.UNSPECIFIED.,.F.,.F.)
B_SPLINE_CURVE_WITH_KNOTS((3,3),(0.140651836354967,0.670383167684795),
 .UNSPECIFIED.)
CURVE()
GEOMETRIC_REPRESENTATION_ITEM()
RATIONAL_B_SPLINE_CURVE((1.11602540378444,1.28867513459481,1.11602540378444))
REPRESENTATION_ITEM('')
);
#263=(
BOUNDED_CURVE()
B_SPLINE_CURVE(2,(#9524,#9525,#9526),.UNSPECIFIED.,.F.,.F.)
B_SPLINE_CURVE_WITH_KNOTS((3,3),(0.140651836354967,0.670383167684795),
 .UNSPECIFIED.)
CURVE()
GEOMETRIC_REPRESENTATION_ITEM()
RATIONAL_B_SPLINE_CURVE((1.11602540378444,1.28867513459481,1.11602540378444))
REPRESENTATION_ITEM('')
);
#264=CONICAL_SURFACE('',#6092,0.27,0.785398163397448);
#265=CONICAL_SURFACE('',#6095,0.576175134594813,1.0471975511966);
#266=CONICAL_SURFACE('',#6307,0.4,0.785398163397448);
#267=CONICAL_SURFACE('',#6311,0.41,0.785398163397448);
#268=CONICAL_SURFACE('',#6315,0.26,0.463647609000806);
#269=CONICAL_SURFACE('',#6319,0.275,0.785398163397449);
#270=CONICAL_SURFACE('',#6330,0.47094010767585,1.0471975511966);
#271=CONICAL_SURFACE('',#6332,0.47094010767585,1.0471975511966);
#272=CONICAL_SURFACE('',#6361,1.025,0.785398163397448);
#273=CONICAL_SURFACE('',#6364,1.025,0.785398163397448);
#274=CONICAL_SURFACE('',#6381,0.325,0.785398163397448);
#275=CONICAL_SURFACE('',#6385,0.335,0.785398163397448);
#276=CONICAL_SURFACE('',#6389,0.21,0.463647609000806);
#277=CONICAL_SURFACE('',#6393,0.18,0.785398163397448);
#278=CONICAL_SURFACE('',#6502,0.325,0.785398163397448);
#279=CONICAL_SURFACE('',#6506,0.335,0.785398163397448);
#280=CONICAL_SURFACE('',#6510,0.21,0.463647609000806);
#281=SHAPE_REPRESENTATION_RELATIONSHIP('SRR','None',#10242,#307);
#282=SHAPE_REPRESENTATION_RELATIONSHIP('SRR','None',#10243,#308);
#283=SHAPE_REPRESENTATION_RELATIONSHIP('SRR','None',#10244,#309);
#284=SHAPE_REPRESENTATION_RELATIONSHIP('SRR','None',#10245,#310);
#285=SHAPE_REPRESENTATION_RELATIONSHIP('SRR','None',#10246,#311);
#286=SHAPE_REPRESENTATION_RELATIONSHIP('SRR','None',#10248,#312);
#287=SHAPE_REPRESENTATION_RELATIONSHIP('SRR','None',#10249,#313);
#288=SHAPE_REPRESENTATION_RELATIONSHIP('SRR','None',#10250,#314);
#289=SHAPE_REPRESENTATION_RELATIONSHIP('SRR','None',#10251,#315);
#290=SHAPE_REPRESENTATION_RELATIONSHIP('SRR','None',#10252,#316);
#291=SHAPE_REPRESENTATION_RELATIONSHIP('SRR','None',#10253,#317);
#292=SHAPE_REPRESENTATION_RELATIONSHIP('SRR','None',#10254,#318);
#293=SHAPE_REPRESENTATION_RELATIONSHIP('SRR','None',#10255,#319);
#294=SHAPE_REPRESENTATION_RELATIONSHIP('SRR','None',#10256,#320);
#295=SHAPE_REPRESENTATION_RELATIONSHIP('SRR','None',#10257,#321);
#296=SHAPE_REPRESENTATION_RELATIONSHIP('SRR','None',#10258,#322);
#297=SHAPE_REPRESENTATION_RELATIONSHIP('SRR','None',#10259,#323);
#298=SHAPE_REPRESENTATION_RELATIONSHIP('SRR','None',#10260,#324);
#299=SHAPE_REPRESENTATION_RELATIONSHIP('SRR','None',#10261,#325);
#300=SHAPE_REPRESENTATION_RELATIONSHIP('SRR','None',#10262,#326);
#301=SHAPE_REPRESENTATION_RELATIONSHIP('SRR','None',#10264,#327);
#302=SHAPE_REPRESENTATION_RELATIONSHIP('SRR','None',#10265,#328);
#303=SHAPE_REPRESENTATION_RELATIONSHIP('SRR','None',#10266,#329);
#304=SHAPE_REPRESENTATION_RELATIONSHIP('SRR','None',#10267,#330);
#305=SHAPE_REPRESENTATION_RELATIONSHIP('SRR','None',#10268,#331);
#306=SHAPE_REPRESENTATION_RELATIONSHIP('SRR','None',#10269,#332);
#307=ADVANCED_BREP_SHAPE_REPRESENTATION('',(#359),#10091);
#308=ADVANCED_BREP_SHAPE_REPRESENTATION('',(#360),#10092);
#309=ADVANCED_BREP_SHAPE_REPRESENTATION('',(#361),#10093);
#310=ADVANCED_BREP_SHAPE_REPRESENTATION('',(#362),#10094);
#311=ADVANCED_BREP_SHAPE_REPRESENTATION('',(#363),#10095);
#312=ADVANCED_BREP_SHAPE_REPRESENTATION('',(#364),#10097);
#313=ADVANCED_BREP_SHAPE_REPRESENTATION('',(#365),#10098);
#314=ADVANCED_BREP_SHAPE_REPRESENTATION('',(#366),#10099);
#315=ADVANCED_BREP_SHAPE_REPRESENTATION('',(#367),#10100);
#316=ADVANCED_BREP_SHAPE_REPRESENTATION('',(#368),#10101);
#317=ADVANCED_BREP_SHAPE_REPRESENTATION('',(#369),#10102);
#318=ADVANCED_BREP_SHAPE_REPRESENTATION('',(#370),#10103);
#319=ADVANCED_BREP_SHAPE_REPRESENTATION('',(#371),#10104);
#320=ADVANCED_BREP_SHAPE_REPRESENTATION('',(#238),#10105);
#321=ADVANCED_BREP_SHAPE_REPRESENTATION('',(#372),#10106);
#322=ADVANCED_BREP_SHAPE_REPRESENTATION('',(#373),#10107);
#323=ADVANCED_BREP_SHAPE_REPRESENTATION('',(#374),#10108);
#324=ADVANCED_BREP_SHAPE_REPRESENTATION('',(#375),#10109);
#325=ADVANCED_BREP_SHAPE_REPRESENTATION('',(#239),#10110);
#326=ADVANCED_BREP_SHAPE_REPRESENTATION('',(#376),#10111);
#327=ADVANCED_BREP_SHAPE_REPRESENTATION('',(#377),#10113);
#328=ADVANCED_BREP_SHAPE_REPRESENTATION('',(#378),#10114);
#329=ADVANCED_BREP_SHAPE_REPRESENTATION('',(#379),#10115);
#330=ADVANCED_BREP_SHAPE_REPRESENTATION('',(#380),#10116);
#331=ADVANCED_BREP_SHAPE_REPRESENTATION('',(#381),#10117);
#332=ADVANCED_BREP_SHAPE_REPRESENTATION('',(#240),#10118);
#333=STYLED_ITEM('',(#10484),#359);
#334=STYLED_ITEM('',(#10484),#360);
#335=STYLED_ITEM('',(#10463),#361);
#336=STYLED_ITEM('',(#10463),#362);
#337=STYLED_ITEM('',(#10477),#363);
#338=STYLED_ITEM('',(#10449),#364);
#339=STYLED_ITEM('',(#10449),#365);
#340=STYLED_ITEM('',(#10449),#366);
#341=STYLED_ITEM('',(#10463),#367);
#342=STYLED_ITEM('',(#10463),#368);
#343=STYLED_ITEM('',(#10456),#369);
#344=STYLED_ITEM('',(#10456),#370);
#345=STYLED_ITEM('',(#10456),#371);
#346=STYLED_ITEM('',(#10477),#238);
#347=STYLED_ITEM('',(#10477),#372);
#348=STYLED_ITEM('',(#10477),#373);
#349=STYLED_ITEM('',(#10456),#374);
#350=STYLED_ITEM('',(#10463),#375);
#351=STYLED_ITEM('',(#10477),#239);
#352=STYLED_ITEM('',(#10470),#376);
#353=STYLED_ITEM('',(#10456),#377);
#354=STYLED_ITEM('',(#10463),#378);
#355=STYLED_ITEM('',(#10484),#379);
#356=STYLED_ITEM('',(#10463),#380);
#357=STYLED_ITEM('',(#10477),#381);
#358=STYLED_ITEM('',(#10477),#240);
#359=MANIFOLD_SOLID_BREP('Body1',#5579);
#360=MANIFOLD_SOLID_BREP('Body1',#5580);
#361=MANIFOLD_SOLID_BREP('Body1',#5581);
#362=MANIFOLD_SOLID_BREP('Body1',#5582);
#363=MANIFOLD_SOLID_BREP('Body1',#5583);
#364=MANIFOLD_SOLID_BREP('Body1',#5584);
#365=MANIFOLD_SOLID_BREP('Body1',#5585);
#366=MANIFOLD_SOLID_BREP('Body1',#5586);
#367=MANIFOLD_SOLID_BREP('Body1',#5587);
#368=MANIFOLD_SOLID_BREP('Body1',#5588);
#369=MANIFOLD_SOLID_BREP('Body1',#5589);
#370=MANIFOLD_SOLID_BREP('Body1',#5590);
#371=MANIFOLD_SOLID_BREP('Body1',#5591);
#372=MANIFOLD_SOLID_BREP('Body1',#5594);
#373=MANIFOLD_SOLID_BREP('Body1',#5595);
#374=MANIFOLD_SOLID_BREP('Body1',#5596);
#375=MANIFOLD_SOLID_BREP('Body1',#5597);
#376=MANIFOLD_SOLID_BREP('Body1',#5600);
#377=MANIFOLD_SOLID_BREP('Body1',#5601);
#378=MANIFOLD_SOLID_BREP('Body1',#5602);
#379=MANIFOLD_SOLID_BREP('Body1',#5603);
#380=MANIFOLD_SOLID_BREP('Body1',#5604);
#381=MANIFOLD_SOLID_BREP('Body1',#5605);
#382=B_SPLINE_CURVE_WITH_KNOTS('',3,(#8408,#8409,#8410,#8411,#8412,#8413,
#8414,#8415),.UNSPECIFIED.,.F.,.F.,(4,2,2,4),(3.10041913490528,3.25801314591541,
3.57457123454079,3.89112932316618),.UNSPECIFIED.);
#383=B_SPLINE_CURVE_WITH_KNOTS('',3,(#8417,#8418,#8419,#8420,#8421,#8422,
#8423,#8424),.UNSPECIFIED.,.F.,.F.,(4,2,2,4),(3.89112932316618,4.20768741179156,
4.52424550041694,4.68183951142707),.UNSPECIFIED.);
#384=B_SPLINE_CURVE_WITH_KNOTS('',3,(#8439,#8440,#8441,#8442,#8443,#8444,
#8445,#8446,#8447,#8448,#8449,#8450,#8451,#8452),.UNSPECIFIED.,.F.,.F.,
(4,2,2,2,2,2,4),(0.506332919461168,0.663926930471297,0.980485019096678,
1.29704310772206,1.61360119634744,1.93015928497282,2.08775329598295),
 .UNSPECIFIED.);
#385=B_SPLINE_CURVE_WITH_KNOTS('',3,(#8463,#8464,#8465,#8466,#8467,#8468,
#8469,#8470),.UNSPECIFIED.,.F.,.F.,(4,2,2,4),(3.10041913490528,3.25801314591541,
3.5745712345408,3.89112932316618),.UNSPECIFIED.);
#386=B_SPLINE_CURVE_WITH_KNOTS('',3,(#8472,#8473,#8474,#8475,#8476,#8477,
#8478,#8479),.UNSPECIFIED.,.F.,.F.,(4,2,2,4),(3.89112932316618,4.20768741179156,
4.52424550041694,4.68183951142707),.UNSPECIFIED.);
#387=B_SPLINE_CURVE_WITH_KNOTS('',3,(#8494,#8495,#8496,#8497,#8498,#8499,
#8500,#8501,#8502,#8503,#8504,#8505,#8506,#8507),.UNSPECIFIED.,.F.,.F.,
(4,2,2,2,2,2,4),(0.506332919461167,0.663926930471296,0.980485019096678,
1.29704310772206,1.61360119634744,1.93015928497282,2.08775329598295),
 .UNSPECIFIED.);
#388=B_SPLINE_CURVE_WITH_KNOTS('',3,(#8518,#8519,#8520,#8521,#8522,#8523,
#8524,#8525),.UNSPECIFIED.,.F.,.F.,(4,2,2,4),(3.10041913490528,3.25801314591541,
3.5745712345408,3.89112932316618),.UNSPECIFIED.);
#389=B_SPLINE_CURVE_WITH_KNOTS('',3,(#8527,#8528,#8529,#8530,#8531,#8532,
#8533,#8534),.UNSPECIFIED.,.F.,.F.,(4,2,2,4),(3.89112932316618,4.20768741179156,
4.52424550041694,4.68183951142707),.UNSPECIFIED.);
#390=B_SPLINE_CURVE_WITH_KNOTS('',3,(#8549,#8550,#8551,#8552,#8553,#8554,
#8555,#8556,#8557,#8558,#8559,#8560,#8561,#8562),.UNSPECIFIED.,.F.,.F.,
(4,2,2,2,2,2,4),(0.506332919461169,0.663926930471296,0.980485019096678,
1.29704310772206,1.61360119634744,1.93015928497282,2.08775329598295),
 .UNSPECIFIED.);
#391=B_SPLINE_CURVE_WITH_KNOTS('',3,(#8570,#8571,#8572,#8573,#8574,#8575,
#8576,#8577),.UNSPECIFIED.,.F.,.F.,(4,2,2,4),(3.10041913490528,3.25801314591541,
3.5745712345408,3.89112932316618),.UNSPECIFIED.);
#392=B_SPLINE_CURVE_WITH_KNOTS('',3,(#8579,#8580,#8581,#8582,#8583,#8584,
#8585,#8586),.UNSPECIFIED.,.F.,.F.,(4,2,2,4),(3.89112932316618,4.20768741179156,
4.52424550041694,4.68183951142707),.UNSPECIFIED.);
#393=B_SPLINE_CURVE_WITH_KNOTS('',3,(#8591,#8592,#8593,#8594,#8595,#8596,
#8597,#8598,#8599,#8600,#8601,#8602,#8603,#8604),.UNSPECIFIED.,.F.,.F.,
(4,2,2,2,2,2,4),(0.506332919461165,0.663926930471296,0.980485019096678,
1.29704310772206,1.61360119634744,1.93015928497282,2.08775329598295),
 .UNSPECIFIED.);
#394=ELLIPSE('',#5919,1.11722871427474,0.789999999999999);
#395=ELLIPSE('',#5920,1.11722871427474,0.789999999999999);
#396=ELLIPSE('',#5922,1.11722871427474,0.789999999999999);
#397=ELLIPSE('',#5924,1.11722871427474,0.789999999999999);
#398=ELLIPSE('',#5926,1.11722871427474,0.789999999999999);
#399=ELLIPSE('',#5927,1.11722871427474,0.789999999999999);
#400=ELLIPSE('',#5930,1.11722871427474,0.789999999999999);
#401=ELLIPSE('',#5931,1.11722871427474,0.789999999999999);
#402=ELLIPSE('',#5935,1.11722871427474,0.79);
#403=ELLIPSE('',#5936,1.11722871427474,0.79);
#404=ELLIPSE('',#5937,1.11722871427475,0.79);
#405=ELLIPSE('',#5938,1.11722871427474,0.79);
#406=ELLIPSE('',#5939,1.11722871427475,0.79);
#407=ELLIPSE('',#5940,1.11722871427475,0.79);
#408=ELLIPSE('',#5941,1.11722871427474,0.789999999999999);
#409=ELLIPSE('',#5942,1.11722871427474,0.789999999999999);
#410=ELLIPSE('',#5943,1.11722871427474,0.789999999999999);
#411=ELLIPSE('',#5944,1.11722871427474,0.789999999999999);
#412=ELLIPSE('',#5945,1.11722871427474,0.789999999999999);
#413=ELLIPSE('',#5946,1.11722871427474,0.789999999999999);
#414=ELLIPSE('',#5947,1.11722871427474,0.789999999999999);
#415=ELLIPSE('',#5948,1.11722871427474,0.789999999999999);
#416=ELLIPSE('',#5949,1.11722871427474,0.789999999999999);
#417=ELLIPSE('',#5950,1.11722871427474,0.789999999999999);
#418=ELLIPSE('',#5951,1.11722871427474,0.789999999999999);
#419=ELLIPSE('',#5952,1.11722871427474,0.789999999999999);
#420=ELLIPSE('',#5953,1.11722871427474,0.789999999999999);
#421=ELLIPSE('',#5954,1.11722871427474,0.789999999999999);
#422=ELLIPSE('',#5955,1.11722871427474,0.789999999999999);
#423=ELLIPSE('',#5956,1.11722871427474,0.789999999999999);
#424=ELLIPSE('',#5957,1.11722871427474,0.79);
#425=ELLIPSE('',#5958,1.11722871427475,0.79);
#426=FACE_BOUND('',#1085,.T.);
#427=FACE_BOUND('',#1088,.T.);
#428=FACE_BOUND('',#1128,.T.);
#429=FACE_BOUND('',#1130,.T.);
#430=FACE_BOUND('',#1131,.T.);
#431=FACE_BOUND('',#1132,.T.);
#432=FACE_BOUND('',#1133,.T.);
#433=FACE_BOUND('',#1135,.T.);
#434=FACE_BOUND('',#1138,.T.);
#435=FACE_BOUND('',#1139,.T.);
#436=FACE_BOUND('',#1141,.T.);
#437=FACE_BOUND('',#1153,.T.);
#438=FACE_BOUND('',#1157,.T.);
#439=FACE_BOUND('',#1161,.T.);
#440=FACE_BOUND('',#1168,.T.);
#441=FACE_BOUND('',#1169,.T.);
#442=FACE_BOUND('',#1170,.T.);
#443=FACE_BOUND('',#1172,.T.);
#444=FACE_BOUND('',#1173,.T.);
#445=FACE_BOUND('',#1174,.T.);
#446=FACE_BOUND('',#1177,.T.);
#447=FACE_BOUND('',#1181,.T.);
#448=FACE_BOUND('',#1185,.T.);
#449=FACE_BOUND('',#1192,.T.);
#450=FACE_BOUND('',#1193,.T.);
#451=FACE_BOUND('',#1194,.T.);
#452=FACE_BOUND('',#1196,.T.);
#453=FACE_BOUND('',#1197,.T.);
#454=FACE_BOUND('',#1198,.T.);
#455=FACE_BOUND('',#1211,.T.);
#456=FACE_BOUND('',#1223,.T.);
#457=FACE_BOUND('',#1224,.T.);
#458=FACE_BOUND('',#1228,.T.);
#459=FACE_BOUND('',#1230,.T.);
#460=FACE_BOUND('',#1232,.T.);
#461=FACE_BOUND('',#1234,.T.);
#462=FACE_BOUND('',#1235,.T.);
#463=FACE_BOUND('',#1236,.T.);
#464=FACE_BOUND('',#1237,.T.);
#465=FACE_BOUND('',#1240,.T.);
#466=FACE_BOUND('',#1241,.T.);
#467=FACE_BOUND('',#1242,.T.);
#468=FACE_BOUND('',#1243,.T.);
#469=FACE_BOUND('',#1244,.T.);
#470=FACE_BOUND('',#1258,.T.);
#471=FACE_BOUND('',#1259,.T.);
#472=FACE_BOUND('',#1263,.T.);
#473=FACE_BOUND('',#1265,.T.);
#474=FACE_BOUND('',#1267,.T.);
#475=FACE_BOUND('',#1269,.T.);
#476=FACE_BOUND('',#1270,.T.);
#477=FACE_BOUND('',#1271,.T.);
#478=FACE_BOUND('',#1272,.T.);
#479=FACE_BOUND('',#1273,.T.);
#480=FACE_BOUND('',#1276,.T.);
#481=FACE_BOUND('',#1277,.T.);
#482=FACE_BOUND('',#1278,.T.);
#483=FACE_BOUND('',#1279,.T.);
#484=FACE_BOUND('',#1291,.T.);
#485=FACE_BOUND('',#1292,.T.);
#486=FACE_BOUND('',#1293,.T.);
#487=FACE_BOUND('',#1294,.T.);
#488=FACE_BOUND('',#1302,.T.);
#489=FACE_BOUND('',#1303,.T.);
#490=FACE_BOUND('',#1304,.T.);
#491=FACE_BOUND('',#1305,.T.);
#492=FACE_BOUND('',#1307,.T.);
#493=FACE_BOUND('',#1310,.T.);
#494=FACE_BOUND('',#1314,.T.);
#495=FACE_BOUND('',#1318,.T.);
#496=FACE_BOUND('',#1322,.T.);
#497=FACE_BOUND('',#1324,.T.);
#498=FACE_BOUND('',#1339,.T.);
#499=FACE_BOUND('',#1340,.T.);
#500=FACE_BOUND('',#1341,.T.);
#501=FACE_BOUND('',#1342,.T.);
#502=FACE_BOUND('',#1343,.T.);
#503=FACE_BOUND('',#1344,.T.);
#504=FACE_BOUND('',#1345,.T.);
#505=FACE_BOUND('',#1347,.T.);
#506=FACE_BOUND('',#1348,.T.);
#507=FACE_BOUND('',#1349,.T.);
#508=FACE_BOUND('',#1350,.T.);
#509=FACE_BOUND('',#1351,.T.);
#510=FACE_BOUND('',#1353,.T.);
#511=FACE_BOUND('',#1357,.T.);
#512=FACE_BOUND('',#1359,.T.);
#513=FACE_BOUND('',#1369,.T.);
#514=FACE_BOUND('',#1377,.T.);
#515=FACE_BOUND('',#1383,.T.);
#516=FACE_BOUND('',#1386,.T.);
#517=FACE_BOUND('',#1397,.T.);
#518=FACE_BOUND('',#1399,.T.);
#519=FACE_BOUND('',#1401,.T.);
#520=FACE_BOUND('',#1403,.T.);
#521=FACE_BOUND('',#1412,.T.);
#522=FACE_BOUND('',#1417,.T.);
#523=FACE_BOUND('',#1422,.T.);
#524=FACE_BOUND('',#1424,.T.);
#525=FACE_BOUND('',#1430,.T.);
#526=FACE_BOUND('',#1453,.T.);
#527=FACE_BOUND('',#1454,.T.);
#528=FACE_BOUND('',#1466,.T.);
#529=FACE_BOUND('',#1478,.T.);
#530=FACE_BOUND('',#1488,.T.);
#531=FACE_BOUND('',#1490,.T.);
#532=FACE_BOUND('',#1494,.T.);
#533=FACE_BOUND('',#1496,.T.);
#534=FACE_BOUND('',#1517,.T.);
#535=PLANE('',#5901);
#536=PLANE('',#5905);
#537=PLANE('',#5909);
#538=PLANE('',#5914);
#539=PLANE('',#5916);
#540=PLANE('',#5933);
#541=PLANE('',#5959);
#542=PLANE('',#5964);
#543=PLANE('',#5965);
#544=PLANE('',#5974);
#545=PLANE('',#5975);
#546=PLANE('',#5980);
#547=PLANE('',#5981);
#548=PLANE('',#5990);
#549=PLANE('',#5991);
#550=PLANE('',#5996);
#551=PLANE('',#5997);
#552=PLANE('',#6006);
#553=PLANE('',#6007);
#554=PLANE('',#6012);
#555=PLANE('',#6013);
#556=PLANE('',#6014);
#557=PLANE('',#6015);
#558=PLANE('',#6016);
#559=PLANE('',#6017);
#560=PLANE('',#6018);
#561=PLANE('',#6020);
#562=PLANE('',#6022);
#563=PLANE('',#6023);
#564=PLANE('',#6024);
#565=PLANE('',#6025);
#566=PLANE('',#6026);
#567=PLANE('',#6027);
#568=PLANE('',#6028);
#569=PLANE('',#6031);
#570=PLANE('',#6036);
#571=PLANE('',#6043);
#572=PLANE('',#6050);
#573=PLANE('',#6054);
#574=PLANE('',#6055);
#575=PLANE('',#6056);
#576=PLANE('',#6057);
#577=PLANE('',#6058);
#578=PLANE('',#6059);
#579=PLANE('',#6064);
#580=PLANE('',#6071);
#581=PLANE('',#6078);
#582=PLANE('',#6082);
#583=PLANE('',#6083);
#584=PLANE('',#6084);
#585=PLANE('',#6085);
#586=PLANE('',#6086);
#587=PLANE('',#6087);
#588=PLANE('',#6094);
#589=PLANE('',#6097);
#590=PLANE('',#6098);
#591=PLANE('',#6099);
#592=PLANE('',#6100);
#593=PLANE('',#6101);
#594=PLANE('',#6102);
#595=PLANE('',#6103);
#596=PLANE('',#6104);
#597=PLANE('',#6110);
#598=PLANE('',#6114);
#599=PLANE('',#6130);
#600=PLANE('',#6132);
#601=PLANE('',#6139);
#602=PLANE('',#6141);
#603=PLANE('',#6144);
#604=PLANE('',#6145);
#605=PLANE('',#6146);
#606=PLANE('',#6147);
#607=PLANE('',#6148);
#608=PLANE('',#6153);
#609=PLANE('',#6157);
#610=PLANE('',#6173);
#611=PLANE('',#6175);
#612=PLANE('',#6182);
#613=PLANE('',#6183);
#614=PLANE('',#6187);
#615=PLANE('',#6188);
#616=PLANE('',#6189);
#617=PLANE('',#6190);
#618=PLANE('',#6191);
#619=PLANE('',#6205);
#620=PLANE('',#6206);
#621=PLANE('',#6207);
#622=PLANE('',#6208);
#623=PLANE('',#6209);
#624=PLANE('',#6211);
#625=PLANE('',#6212);
#626=PLANE('',#6215);
#627=PLANE('',#6216);
#628=PLANE('',#6217);
#629=PLANE('',#6218);
#630=PLANE('',#6220);
#631=PLANE('',#6225);
#632=PLANE('',#6231);
#633=PLANE('',#6240);
#634=PLANE('',#6247);
#635=PLANE('',#6248);
#636=PLANE('',#6253);
#637=PLANE('',#6257);
#638=PLANE('',#6273);
#639=PLANE('',#6274);
#640=PLANE('',#6275);
#641=PLANE('',#6276);
#642=PLANE('',#6277);
#643=PLANE('',#6278);
#644=PLANE('',#6288);
#645=PLANE('',#6289);
#646=PLANE('',#6291);
#647=PLANE('',#6292);
#648=PLANE('',#6293);
#649=PLANE('',#6294);
#650=PLANE('',#6295);
#651=PLANE('',#6296);
#652=PLANE('',#6297);
#653=PLANE('',#6298);
#654=PLANE('',#6299);
#655=PLANE('',#6304);
#656=PLANE('',#6305);
#657=PLANE('',#6313);
#658=PLANE('',#6324);
#659=PLANE('',#6328);
#660=PLANE('',#6334);
#661=PLANE('',#6335);
#662=PLANE('',#6336);
#663=PLANE('',#6340);
#664=PLANE('',#6341);
#665=PLANE('',#6342);
#666=PLANE('',#6343);
#667=PLANE('',#6344);
#668=PLANE('',#6346);
#669=PLANE('',#6348);
#670=PLANE('',#6350);
#671=PLANE('',#6351);
#672=PLANE('',#6352);
#673=PLANE('',#6353);
#674=PLANE('',#6354);
#675=PLANE('',#6355);
#676=PLANE('',#6358);
#677=PLANE('',#6366);
#678=PLANE('',#6376);
#679=PLANE('',#6377);
#680=PLANE('',#6379);
#681=PLANE('',#6387);
#682=PLANE('',#6395);
#683=PLANE('',#6396);
#684=PLANE('',#6397);
#685=PLANE('',#6398);
#686=PLANE('',#6399);
#687=PLANE('',#6400);
#688=PLANE('',#6401);
#689=PLANE('',#6402);
#690=PLANE('',#6403);
#691=PLANE('',#6408);
#692=PLANE('',#6409);
#693=PLANE('',#6412);
#694=PLANE('',#6414);
#695=PLANE('',#6417);
#696=PLANE('',#6419);
#697=PLANE('',#6421);
#698=PLANE('',#6431);
#699=PLANE('',#6432);
#700=PLANE('',#6434);
#701=PLANE('',#6436);
#702=PLANE('',#6438);
#703=PLANE('',#6440);
#704=PLANE('',#6441);
#705=PLANE('',#6442);
#706=PLANE('',#6443);
#707=PLANE('',#6444);
#708=PLANE('',#6445);
#709=PLANE('',#6447);
#710=PLANE('',#6450);
#711=PLANE('',#6452);
#712=PLANE('',#6454);
#713=PLANE('',#6455);
#714=PLANE('',#6456);
#715=PLANE('',#6457);
#716=PLANE('',#6458);
#717=PLANE('',#6461);
#718=PLANE('',#6463);
#719=PLANE('',#6464);
#720=PLANE('',#6465);
#721=PLANE('',#6466);
#722=PLANE('',#6467);
#723=PLANE('',#6468);
#724=PLANE('',#6469);
#725=PLANE('',#6470);
#726=PLANE('',#6471);
#727=PLANE('',#6472);
#728=PLANE('',#6480);
#729=PLANE('',#6481);
#730=PLANE('',#6483);
#731=PLANE('',#6484);
#732=PLANE('',#6485);
#733=PLANE('',#6486);
#734=PLANE('',#6487);
#735=PLANE('',#6488);
#736=PLANE('',#6490);
#737=PLANE('',#6491);
#738=PLANE('',#6492);
#739=PLANE('',#6493);
#740=PLANE('',#6494);
#741=PLANE('',#6495);
#742=PLANE('',#6496);
#743=PLANE('',#6497);
#744=PLANE('',#6498);
#745=PLANE('',#6500);
#746=PLANE('',#6508);
#747=FACE_OUTER_BOUND('',#1079,.T.);
#748=FACE_OUTER_BOUND('',#1080,.T.);
#749=FACE_OUTER_BOUND('',#1081,.T.);
#750=FACE_OUTER_BOUND('',#1082,.T.);
#751=FACE_OUTER_BOUND('',#1083,.T.);
#752=FACE_OUTER_BOUND('',#1084,.T.);
#753=FACE_OUTER_BOUND('',#1086,.T.);
#754=FACE_OUTER_BOUND('',#1087,.T.);
#755=FACE_OUTER_BOUND('',#1089,.T.);
#756=FACE_OUTER_BOUND('',#1090,.T.);
#757=FACE_OUTER_BOUND('',#1091,.T.);
#758=FACE_OUTER_BOUND('',#1092,.T.);
#759=FACE_OUTER_BOUND('',#1093,.T.);
#760=FACE_OUTER_BOUND('',#1094,.T.);
#761=FACE_OUTER_BOUND('',#1095,.T.);
#762=FACE_OUTER_BOUND('',#1096,.T.);
#763=FACE_OUTER_BOUND('',#1097,.T.);
#764=FACE_OUTER_BOUND('',#1098,.T.);
#765=FACE_OUTER_BOUND('',#1099,.T.);
#766=FACE_OUTER_BOUND('',#1100,.T.);
#767=FACE_OUTER_BOUND('',#1101,.T.);
#768=FACE_OUTER_BOUND('',#1102,.T.);
#769=FACE_OUTER_BOUND('',#1103,.T.);
#770=FACE_OUTER_BOUND('',#1104,.T.);
#771=FACE_OUTER_BOUND('',#1105,.T.);
#772=FACE_OUTER_BOUND('',#1106,.T.);
#773=FACE_OUTER_BOUND('',#1107,.T.);
#774=FACE_OUTER_BOUND('',#1108,.T.);
#775=FACE_OUTER_BOUND('',#1109,.T.);
#776=FACE_OUTER_BOUND('',#1110,.T.);
#777=FACE_OUTER_BOUND('',#1111,.T.);
#778=FACE_OUTER_BOUND('',#1112,.T.);
#779=FACE_OUTER_BOUND('',#1113,.T.);
#780=FACE_OUTER_BOUND('',#1114,.T.);
#781=FACE_OUTER_BOUND('',#1115,.T.);
#782=FACE_OUTER_BOUND('',#1116,.T.);
#783=FACE_OUTER_BOUND('',#1117,.T.);
#784=FACE_OUTER_BOUND('',#1118,.T.);
#785=FACE_OUTER_BOUND('',#1119,.T.);
#786=FACE_OUTER_BOUND('',#1120,.T.);
#787=FACE_OUTER_BOUND('',#1121,.T.);
#788=FACE_OUTER_BOUND('',#1122,.T.);
#789=FACE_OUTER_BOUND('',#1123,.T.);
#790=FACE_OUTER_BOUND('',#1124,.T.);
#791=FACE_OUTER_BOUND('',#1125,.T.);
#792=FACE_OUTER_BOUND('',#1126,.T.);
#793=FACE_OUTER_BOUND('',#1127,.T.);
#794=FACE_OUTER_BOUND('',#1129,.T.);
#795=FACE_OUTER_BOUND('',#1134,.T.);
#796=FACE_OUTER_BOUND('',#1136,.T.);
#797=FACE_OUTER_BOUND('',#1137,.T.);
#798=FACE_OUTER_BOUND('',#1140,.T.);
#799=FACE_OUTER_BOUND('',#1142,.T.);
#800=FACE_OUTER_BOUND('',#1143,.T.);
#801=FACE_OUTER_BOUND('',#1144,.T.);
#802=FACE_OUTER_BOUND('',#1145,.T.);
#803=FACE_OUTER_BOUND('',#1146,.T.);
#804=FACE_OUTER_BOUND('',#1147,.T.);
#805=FACE_OUTER_BOUND('',#1148,.T.);
#806=FACE_OUTER_BOUND('',#1149,.T.);
#807=FACE_OUTER_BOUND('',#1150,.T.);
#808=FACE_OUTER_BOUND('',#1151,.T.);
#809=FACE_OUTER_BOUND('',#1152,.T.);
#810=FACE_OUTER_BOUND('',#1154,.T.);
#811=FACE_OUTER_BOUND('',#1155,.T.);
#812=FACE_OUTER_BOUND('',#1156,.T.);
#813=FACE_OUTER_BOUND('',#1158,.T.);
#814=FACE_OUTER_BOUND('',#1159,.T.);
#815=FACE_OUTER_BOUND('',#1160,.T.);
#816=FACE_OUTER_BOUND('',#1162,.T.);
#817=FACE_OUTER_BOUND('',#1163,.T.);
#818=FACE_OUTER_BOUND('',#1164,.T.);
#819=FACE_OUTER_BOUND('',#1165,.T.);
#820=FACE_OUTER_BOUND('',#1166,.T.);
#821=FACE_OUTER_BOUND('',#1167,.T.);
#822=FACE_OUTER_BOUND('',#1171,.T.);
#823=FACE_OUTER_BOUND('',#1175,.T.);
#824=FACE_OUTER_BOUND('',#1176,.T.);
#825=FACE_OUTER_BOUND('',#1178,.T.);
#826=FACE_OUTER_BOUND('',#1179,.T.);
#827=FACE_OUTER_BOUND('',#1180,.T.);
#828=FACE_OUTER_BOUND('',#1182,.T.);
#829=FACE_OUTER_BOUND('',#1183,.T.);
#830=FACE_OUTER_BOUND('',#1184,.T.);
#831=FACE_OUTER_BOUND('',#1186,.T.);
#832=FACE_OUTER_BOUND('',#1187,.T.);
#833=FACE_OUTER_BOUND('',#1188,.T.);
#834=FACE_OUTER_BOUND('',#1189,.T.);
#835=FACE_OUTER_BOUND('',#1190,.T.);
#836=FACE_OUTER_BOUND('',#1191,.T.);
#837=FACE_OUTER_BOUND('',#1195,.T.);
#838=FACE_OUTER_BOUND('',#1199,.T.);
#839=FACE_OUTER_BOUND('',#1200,.T.);
#840=FACE_OUTER_BOUND('',#1201,.T.);
#841=FACE_OUTER_BOUND('',#1202,.T.);
#842=FACE_OUTER_BOUND('',#1203,.T.);
#843=FACE_OUTER_BOUND('',#1204,.T.);
#844=FACE_OUTER_BOUND('',#1205,.T.);
#845=FACE_OUTER_BOUND('',#1206,.T.);
#846=FACE_OUTER_BOUND('',#1207,.T.);
#847=FACE_OUTER_BOUND('',#1208,.T.);
#848=FACE_OUTER_BOUND('',#1209,.T.);
#849=FACE_OUTER_BOUND('',#1210,.T.);
#850=FACE_OUTER_BOUND('',#1212,.T.);
#851=FACE_OUTER_BOUND('',#1213,.T.);
#852=FACE_OUTER_BOUND('',#1214,.T.);
#853=FACE_OUTER_BOUND('',#1215,.T.);
#854=FACE_OUTER_BOUND('',#1216,.T.);
#855=FACE_OUTER_BOUND('',#1217,.T.);
#856=FACE_OUTER_BOUND('',#1218,.T.);
#857=FACE_OUTER_BOUND('',#1219,.T.);
#858=FACE_OUTER_BOUND('',#1220,.T.);
#859=FACE_OUTER_BOUND('',#1221,.T.);
#860=FACE_OUTER_BOUND('',#1222,.T.);
#861=FACE_OUTER_BOUND('',#1225,.T.);
#862=FACE_OUTER_BOUND('',#1226,.T.);
#863=FACE_OUTER_BOUND('',#1227,.T.);
#864=FACE_OUTER_BOUND('',#1229,.T.);
#865=FACE_OUTER_BOUND('',#1231,.T.);
#866=FACE_OUTER_BOUND('',#1233,.T.);
#867=FACE_OUTER_BOUND('',#1238,.T.);
#868=FACE_OUTER_BOUND('',#1239,.T.);
#869=FACE_OUTER_BOUND('',#1245,.T.);
#870=FACE_OUTER_BOUND('',#1246,.T.);
#871=FACE_OUTER_BOUND('',#1247,.T.);
#872=FACE_OUTER_BOUND('',#1248,.T.);
#873=FACE_OUTER_BOUND('',#1249,.T.);
#874=FACE_OUTER_BOUND('',#1250,.T.);
#875=FACE_OUTER_BOUND('',#1251,.T.);
#876=FACE_OUTER_BOUND('',#1252,.T.);
#877=FACE_OUTER_BOUND('',#1253,.T.);
#878=FACE_OUTER_BOUND('',#1254,.T.);
#879=FACE_OUTER_BOUND('',#1255,.T.);
#880=FACE_OUTER_BOUND('',#1256,.T.);
#881=FACE_OUTER_BOUND('',#1257,.T.);
#882=FACE_OUTER_BOUND('',#1260,.T.);
#883=FACE_OUTER_BOUND('',#1261,.T.);
#884=FACE_OUTER_BOUND('',#1262,.T.);
#885=FACE_OUTER_BOUND('',#1264,.T.);
#886=FACE_OUTER_BOUND('',#1266,.T.);
#887=FACE_OUTER_BOUND('',#1268,.T.);
#888=FACE_OUTER_BOUND('',#1274,.T.);
#889=FACE_OUTER_BOUND('',#1275,.T.);
#890=FACE_OUTER_BOUND('',#1280,.T.);
#891=FACE_OUTER_BOUND('',#1281,.T.);
#892=FACE_OUTER_BOUND('',#1282,.T.);
#893=FACE_OUTER_BOUND('',#1283,.T.);
#894=FACE_OUTER_BOUND('',#1284,.T.);
#895=FACE_OUTER_BOUND('',#1285,.T.);
#896=FACE_OUTER_BOUND('',#1286,.T.);
#897=FACE_OUTER_BOUND('',#1287,.T.);
#898=FACE_OUTER_BOUND('',#1288,.T.);
#899=FACE_OUTER_BOUND('',#1289,.T.);
#900=FACE_OUTER_BOUND('',#1290,.T.);
#901=FACE_OUTER_BOUND('',#1295,.T.);
#902=FACE_OUTER_BOUND('',#1296,.T.);
#903=FACE_OUTER_BOUND('',#1297,.T.);
#904=FACE_OUTER_BOUND('',#1298,.T.);
#905=FACE_OUTER_BOUND('',#1299,.T.);
#906=FACE_OUTER_BOUND('',#1300,.T.);
#907=FACE_OUTER_BOUND('',#1301,.T.);
#908=FACE_OUTER_BOUND('',#1306,.T.);
#909=FACE_OUTER_BOUND('',#1308,.T.);
#910=FACE_OUTER_BOUND('',#1309,.T.);
#911=FACE_OUTER_BOUND('',#1311,.T.);
#912=FACE_OUTER_BOUND('',#1312,.T.);
#913=FACE_OUTER_BOUND('',#1313,.T.);
#914=FACE_OUTER_BOUND('',#1315,.T.);
#915=FACE_OUTER_BOUND('',#1316,.T.);
#916=FACE_OUTER_BOUND('',#1317,.T.);
#917=FACE_OUTER_BOUND('',#1319,.T.);
#918=FACE_OUTER_BOUND('',#1320,.T.);
#919=FACE_OUTER_BOUND('',#1321,.T.);
#920=FACE_OUTER_BOUND('',#1323,.T.);
#921=FACE_OUTER_BOUND('',#1325,.T.);
#922=FACE_OUTER_BOUND('',#1326,.T.);
#923=FACE_OUTER_BOUND('',#1327,.T.);
#924=FACE_OUTER_BOUND('',#1328,.T.);
#925=FACE_OUTER_BOUND('',#1329,.T.);
#926=FACE_OUTER_BOUND('',#1330,.T.);
#927=FACE_OUTER_BOUND('',#1331,.T.);
#928=FACE_OUTER_BOUND('',#1332,.T.);
#929=FACE_OUTER_BOUND('',#1333,.T.);
#930=FACE_OUTER_BOUND('',#1334,.T.);
#931=FACE_OUTER_BOUND('',#1335,.T.);
#932=FACE_OUTER_BOUND('',#1336,.T.);
#933=FACE_OUTER_BOUND('',#1337,.T.);
#934=FACE_OUTER_BOUND('',#1338,.T.);
#935=FACE_OUTER_BOUND('',#1346,.T.);
#936=FACE_OUTER_BOUND('',#1352,.T.);
#937=FACE_OUTER_BOUND('',#1354,.T.);
#938=FACE_OUTER_BOUND('',#1355,.T.);
#939=FACE_OUTER_BOUND('',#1356,.T.);
#940=FACE_OUTER_BOUND('',#1358,.T.);
#941=FACE_OUTER_BOUND('',#1360,.T.);
#942=FACE_OUTER_BOUND('',#1361,.T.);
#943=FACE_OUTER_BOUND('',#1362,.T.);
#944=FACE_OUTER_BOUND('',#1363,.T.);
#945=FACE_OUTER_BOUND('',#1364,.T.);
#946=FACE_OUTER_BOUND('',#1365,.T.);
#947=FACE_OUTER_BOUND('',#1366,.T.);
#948=FACE_OUTER_BOUND('',#1367,.T.);
#949=FACE_OUTER_BOUND('',#1368,.T.);
#950=FACE_OUTER_BOUND('',#1370,.T.);
#951=FACE_OUTER_BOUND('',#1371,.T.);
#952=FACE_OUTER_BOUND('',#1372,.T.);
#953=FACE_OUTER_BOUND('',#1373,.T.);
#954=FACE_OUTER_BOUND('',#1374,.T.);
#955=FACE_OUTER_BOUND('',#1375,.T.);
#956=FACE_OUTER_BOUND('',#1376,.T.);
#957=FACE_OUTER_BOUND('',#1378,.T.);
#958=FACE_OUTER_BOUND('',#1379,.T.);
#959=FACE_OUTER_BOUND('',#1380,.T.);
#960=FACE_OUTER_BOUND('',#1381,.T.);
#961=FACE_OUTER_BOUND('',#1382,.T.);
#962=FACE_OUTER_BOUND('',#1384,.T.);
#963=FACE_OUTER_BOUND('',#1385,.T.);
#964=FACE_OUTER_BOUND('',#1387,.T.);
#965=FACE_OUTER_BOUND('',#1388,.T.);
#966=FACE_OUTER_BOUND('',#1389,.T.);
#967=FACE_OUTER_BOUND('',#1390,.T.);
#968=FACE_OUTER_BOUND('',#1391,.T.);
#969=FACE_OUTER_BOUND('',#1392,.T.);
#970=FACE_OUTER_BOUND('',#1393,.T.);
#971=FACE_OUTER_BOUND('',#1394,.T.);
#972=FACE_OUTER_BOUND('',#1395,.T.);
#973=FACE_OUTER_BOUND('',#1396,.T.);
#974=FACE_OUTER_BOUND('',#1398,.T.);
#975=FACE_OUTER_BOUND('',#1400,.T.);
#976=FACE_OUTER_BOUND('',#1402,.T.);
#977=FACE_OUTER_BOUND('',#1404,.T.);
#978=FACE_OUTER_BOUND('',#1405,.T.);
#979=FACE_OUTER_BOUND('',#1406,.T.);
#980=FACE_OUTER_BOUND('',#1407,.T.);
#981=FACE_OUTER_BOUND('',#1408,.T.);
#982=FACE_OUTER_BOUND('',#1409,.T.);
#983=FACE_OUTER_BOUND('',#1410,.T.);
#984=FACE_OUTER_BOUND('',#1411,.T.);
#985=FACE_OUTER_BOUND('',#1413,.T.);
#986=FACE_OUTER_BOUND('',#1414,.T.);
#987=FACE_OUTER_BOUND('',#1415,.T.);
#988=FACE_OUTER_BOUND('',#1416,.T.);
#989=FACE_OUTER_BOUND('',#1418,.T.);
#990=FACE_OUTER_BOUND('',#1419,.T.);
#991=FACE_OUTER_BOUND('',#1420,.T.);
#992=FACE_OUTER_BOUND('',#1421,.T.);
#993=FACE_OUTER_BOUND('',#1423,.T.);
#994=FACE_OUTER_BOUND('',#1425,.T.);
#995=FACE_OUTER_BOUND('',#1426,.T.);
#996=FACE_OUTER_BOUND('',#1427,.T.);
#997=FACE_OUTER_BOUND('',#1428,.T.);
#998=FACE_OUTER_BOUND('',#1429,.T.);
#999=FACE_OUTER_BOUND('',#1431,.T.);
#1000=FACE_OUTER_BOUND('',#1432,.T.);
#1001=FACE_OUTER_BOUND('',#1433,.T.);
#1002=FACE_OUTER_BOUND('',#1434,.T.);
#1003=FACE_OUTER_BOUND('',#1435,.T.);
#1004=FACE_OUTER_BOUND('',#1436,.T.);
#1005=FACE_OUTER_BOUND('',#1437,.T.);
#1006=FACE_OUTER_BOUND('',#1438,.T.);
#1007=FACE_OUTER_BOUND('',#1439,.T.);
#1008=FACE_OUTER_BOUND('',#1440,.T.);
#1009=FACE_OUTER_BOUND('',#1441,.T.);
#1010=FACE_OUTER_BOUND('',#1442,.T.);
#1011=FACE_OUTER_BOUND('',#1443,.T.);
#1012=FACE_OUTER_BOUND('',#1444,.T.);
#1013=FACE_OUTER_BOUND('',#1445,.T.);
#1014=FACE_OUTER_BOUND('',#1446,.T.);
#1015=FACE_OUTER_BOUND('',#1447,.T.);
#1016=FACE_OUTER_BOUND('',#1448,.T.);
#1017=FACE_OUTER_BOUND('',#1449,.T.);
#1018=FACE_OUTER_BOUND('',#1450,.T.);
#1019=FACE_OUTER_BOUND('',#1451,.T.);
#1020=FACE_OUTER_BOUND('',#1452,.T.);
#1021=FACE_OUTER_BOUND('',#1455,.T.);
#1022=FACE_OUTER_BOUND('',#1456,.T.);
#1023=FACE_OUTER_BOUND('',#1457,.T.);
#1024=FACE_OUTER_BOUND('',#1458,.T.);
#1025=FACE_OUTER_BOUND('',#1459,.T.);
#1026=FACE_OUTER_BOUND('',#1460,.T.);
#1027=FACE_OUTER_BOUND('',#1461,.T.);
#1028=FACE_OUTER_BOUND('',#1462,.T.);
#1029=FACE_OUTER_BOUND('',#1463,.T.);
#1030=FACE_OUTER_BOUND('',#1464,.T.);
#1031=FACE_OUTER_BOUND('',#1465,.T.);
#1032=FACE_OUTER_BOUND('',#1467,.T.);
#1033=FACE_OUTER_BOUND('',#1468,.T.);
#1034=FACE_OUTER_BOUND('',#1469,.T.);
#1035=FACE_OUTER_BOUND('',#1470,.T.);
#1036=FACE_OUTER_BOUND('',#1471,.T.);
#1037=FACE_OUTER_BOUND('',#1472,.T.);
#1038=FACE_OUTER_BOUND('',#1473,.T.);
#1039=FACE_OUTER_BOUND('',#1474,.T.);
#1040=FACE_OUTER_BOUND('',#1475,.T.);
#1041=FACE_OUTER_BOUND('',#1476,.T.);
#1042=FACE_OUTER_BOUND('',#1477,.T.);
#1043=FACE_OUTER_BOUND('',#1479,.T.);
#1044=FACE_OUTER_BOUND('',#1480,.T.);
#1045=FACE_OUTER_BOUND('',#1481,.T.);
#1046=FACE_OUTER_BOUND('',#1482,.T.);
#1047=FACE_OUTER_BOUND('',#1483,.T.);
#1048=FACE_OUTER_BOUND('',#1484,.T.);
#1049=FACE_OUTER_BOUND('',#1485,.T.);
#1050=FACE_OUTER_BOUND('',#1486,.T.);
#1051=FACE_OUTER_BOUND('',#1487,.T.);
#1052=FACE_OUTER_BOUND('',#1489,.T.);
#1053=FACE_OUTER_BOUND('',#1491,.T.);
#1054=FACE_OUTER_BOUND('',#1492,.T.);
#1055=FACE_OUTER_BOUND('',#1493,.T.);
#1056=FACE_OUTER_BOUND('',#1495,.T.);
#1057=FACE_OUTER_BOUND('',#1497,.T.);
#1058=FACE_OUTER_BOUND('',#1498,.T.);
#1059=FACE_OUTER_BOUND('',#1499,.T.);
#1060=FACE_OUTER_BOUND('',#1500,.T.);
#1061=FACE_OUTER_BOUND('',#1501,.T.);
#1062=FACE_OUTER_BOUND('',#1502,.T.);
#1063=FACE_OUTER_BOUND('',#1503,.T.);
#1064=FACE_OUTER_BOUND('',#1504,.T.);
#1065=FACE_OUTER_BOUND('',#1505,.T.);
#1066=FACE_OUTER_BOUND('',#1506,.T.);
#1067=FACE_OUTER_BOUND('',#1507,.T.);
#1068=FACE_OUTER_BOUND('',#1508,.T.);
#1069=FACE_OUTER_BOUND('',#1509,.T.);
#1070=FACE_OUTER_BOUND('',#1510,.T.);
#1071=FACE_OUTER_BOUND('',#1511,.T.);
#1072=FACE_OUTER_BOUND('',#1512,.T.);
#1073=FACE_OUTER_BOUND('',#1513,.T.);
#1074=FACE_OUTER_BOUND('',#1514,.T.);
#1075=FACE_OUTER_BOUND('',#1515,.T.);
#1076=FACE_OUTER_BOUND('',#1516,.T.);
#1077=FACE_OUTER_BOUND('',#1518,.T.);
#1078=FACE_OUTER_BOUND('',#1519,.T.);
#1079=EDGE_LOOP('',(#3741,#3742,#3743,#3744));
#1080=EDGE_LOOP('',(#3745));
#1081=EDGE_LOOP('',(#3746,#3747,#3748,#3749));
#1082=EDGE_LOOP('',(#3750));
#1083=EDGE_LOOP('',(#3751,#3752,#3753,#3754));
#1084=EDGE_LOOP('',(#3755));
#1085=EDGE_LOOP('',(#3756));
#1086=EDGE_LOOP('',(#3757,#3758,#3759,#3760));
#1087=EDGE_LOOP('',(#3761));
#1088=EDGE_LOOP('',(#3762));
#1089=EDGE_LOOP('',(#3763,#3764));
#1090=EDGE_LOOP('',(#3765,#3766,#3767));
#1091=EDGE_LOOP('',(#3768,#3769,#3770));
#1092=EDGE_LOOP('',(#3771,#3772,#3773));
#1093=EDGE_LOOP('',(#3774,#3775,#3776));
#1094=EDGE_LOOP('',(#3777,#3778));
#1095=EDGE_LOOP('',(#3779,#3780,#3781,#3782,#3783,#3784,#3785,#3786,#3787,
#3788,#3789,#3790,#3791,#3792,#3793,#3794,#3795,#3796,#3797,#3798,#3799,
#3800,#3801,#3802,#3803,#3804,#3805,#3806,#3807,#3808,#3809,#3810,#3811,
#3812,#3813,#3814,#3815,#3816,#3817,#3818,#3819,#3820,#3821,#3822,#3823,
#3824,#3825,#3826,#3827,#3828,#3829,#3830,#3831,#3832,#3833,#3834,#3835,
#3836,#3837,#3838,#3839,#3840,#3841,#3842,#3843,#3844,#3845,#3846,#3847,
#3848,#3849,#3850,#3851,#3852,#3853,#3854,#3855,#3856,#3857,#3858));
#1096=EDGE_LOOP('',(#3859,#3860,#3861,#3862));
#1097=EDGE_LOOP('',(#3863,#3864,#3865,#3866,#3867,#3868,#3869,#3870));
#1098=EDGE_LOOP('',(#3871,#3872,#3873,#3874));
#1099=EDGE_LOOP('',(#3875,#3876));
#1100=EDGE_LOOP('',(#3877,#3878,#3879));
#1101=EDGE_LOOP('',(#3880,#3881,#3882));
#1102=EDGE_LOOP('',(#3883,#3884,#3885));
#1103=EDGE_LOOP('',(#3886,#3887,#3888));
#1104=EDGE_LOOP('',(#3889,#3890));
#1105=EDGE_LOOP('',(#3891,#3892,#3893,#3894));
#1106=EDGE_LOOP('',(#3895,#3896,#3897,#3898,#3899,#3900,#3901,#3902));
#1107=EDGE_LOOP('',(#3903,#3904,#3905,#3906));
#1108=EDGE_LOOP('',(#3907,#3908));
#1109=EDGE_LOOP('',(#3909,#3910,#3911));
#1110=EDGE_LOOP('',(#3912,#3913,#3914));
#1111=EDGE_LOOP('',(#3915,#3916,#3917));
#1112=EDGE_LOOP('',(#3918,#3919,#3920));
#1113=EDGE_LOOP('',(#3921,#3922));
#1114=EDGE_LOOP('',(#3923,#3924,#3925,#3926));
#1115=EDGE_LOOP('',(#3927,#3928,#3929,#3930,#3931,#3932,#3933,#3934));
#1116=EDGE_LOOP('',(#3935,#3936,#3937,#3938));
#1117=EDGE_LOOP('',(#3939,#3940));
#1118=EDGE_LOOP('',(#3941,#3942,#3943));
#1119=EDGE_LOOP('',(#3944,#3945,#3946));
#1120=EDGE_LOOP('',(#3947,#3948,#3949));
#1121=EDGE_LOOP('',(#3950,#3951,#3952));
#1122=EDGE_LOOP('',(#3953,#3954));
#1123=EDGE_LOOP('',(#3955,#3956,#3957,#3958));
#1124=EDGE_LOOP('',(#3959,#3960,#3961,#3962,#3963,#3964,#3965,#3966));
#1125=EDGE_LOOP('',(#3967,#3968,#3969,#3970));
#1126=EDGE_LOOP('',(#3971,#3972,#3973,#3974));
#1127=EDGE_LOOP('',(#3975,#3976,#3977,#3978));
#1128=EDGE_LOOP('',(#3979));
#1129=EDGE_LOOP('',(#3980,#3981,#3982,#3983));
#1130=EDGE_LOOP('',(#3984));
#1131=EDGE_LOOP('',(#3985));
#1132=EDGE_LOOP('',(#3986));
#1133=EDGE_LOOP('',(#3987));
#1134=EDGE_LOOP('',(#3988,#3989,#3990,#3991));
#1135=EDGE_LOOP('',(#3992));
#1136=EDGE_LOOP('',(#3993,#3994,#3995,#3996));
#1137=EDGE_LOOP('',(#3997,#3998,#3999,#4000));
#1138=EDGE_LOOP('',(#4001));
#1139=EDGE_LOOP('',(#4002));
#1140=EDGE_LOOP('',(#4003,#4004,#4005,#4006,#4007,#4008));
#1141=EDGE_LOOP('',(#4009));
#1142=EDGE_LOOP('',(#4010,#4011,#4012,#4013));
#1143=EDGE_LOOP('',(#4014,#4015,#4016,#4017));
#1144=EDGE_LOOP('',(#4018,#4019,#4020,#4021));
#1145=EDGE_LOOP('',(#4022,#4023,#4024,#4025));
#1146=EDGE_LOOP('',(#4026,#4027,#4028,#4029));
#1147=EDGE_LOOP('',(#4030,#4031,#4032,#4033));
#1148=EDGE_LOOP('',(#4034,#4035,#4036,#4037,#4038,#4039));
#1149=EDGE_LOOP('',(#4040,#4041,#4042,#4043));
#1150=EDGE_LOOP('',(#4044));
#1151=EDGE_LOOP('',(#4045,#4046,#4047,#4048));
#1152=EDGE_LOOP('',(#4049));
#1153=EDGE_LOOP('',(#4050));
#1154=EDGE_LOOP('',(#4051,#4052,#4053,#4054));
#1155=EDGE_LOOP('',(#4055,#4056,#4057,#4058));
#1156=EDGE_LOOP('',(#4059));
#1157=EDGE_LOOP('',(#4060));
#1158=EDGE_LOOP('',(#4061,#4062,#4063,#4064));
#1159=EDGE_LOOP('',(#4065,#4066,#4067,#4068));
#1160=EDGE_LOOP('',(#4069));
#1161=EDGE_LOOP('',(#4070));
#1162=EDGE_LOOP('',(#4071,#4072,#4073,#4074));
#1163=EDGE_LOOP('',(#4075,#4076,#4077,#4078));
#1164=EDGE_LOOP('',(#4079,#4080,#4081,#4082));
#1165=EDGE_LOOP('',(#4083,#4084,#4085,#4086));
#1166=EDGE_LOOP('',(#4087,#4088,#4089,#4090));
#1167=EDGE_LOOP('',(#4091,#4092,#4093,#4094));
#1168=EDGE_LOOP('',(#4095));
#1169=EDGE_LOOP('',(#4096));
#1170=EDGE_LOOP('',(#4097));
#1171=EDGE_LOOP('',(#4098,#4099,#4100,#4101));
#1172=EDGE_LOOP('',(#4102));
#1173=EDGE_LOOP('',(#4103));
#1174=EDGE_LOOP('',(#4104));
#1175=EDGE_LOOP('',(#4105,#4106,#4107,#4108));
#1176=EDGE_LOOP('',(#4109));
#1177=EDGE_LOOP('',(#4110));
#1178=EDGE_LOOP('',(#4111,#4112,#4113,#4114));
#1179=EDGE_LOOP('',(#4115,#4116,#4117,#4118));
#1180=EDGE_LOOP('',(#4119));
#1181=EDGE_LOOP('',(#4120));
#1182=EDGE_LOOP('',(#4121,#4122,#4123,#4124));
#1183=EDGE_LOOP('',(#4125,#4126,#4127,#4128));
#1184=EDGE_LOOP('',(#4129));
#1185=EDGE_LOOP('',(#4130));
#1186=EDGE_LOOP('',(#4131,#4132,#4133,#4134));
#1187=EDGE_LOOP('',(#4135,#4136,#4137,#4138));
#1188=EDGE_LOOP('',(#4139,#4140,#4141,#4142));
#1189=EDGE_LOOP('',(#4143,#4144,#4145,#4146));
#1190=EDGE_LOOP('',(#4147,#4148,#4149,#4150));
#1191=EDGE_LOOP('',(#4151,#4152,#4153,#4154));
#1192=EDGE_LOOP('',(#4155));
#1193=EDGE_LOOP('',(#4156));
#1194=EDGE_LOOP('',(#4157));
#1195=EDGE_LOOP('',(#4158,#4159,#4160,#4161));
#1196=EDGE_LOOP('',(#4162));
#1197=EDGE_LOOP('',(#4163));
#1198=EDGE_LOOP('',(#4164));
#1199=EDGE_LOOP('',(#4165,#4166,#4167,#4168));
#1200=EDGE_LOOP('',(#4169,#4170,#4171,#4172));
#1201=EDGE_LOOP('',(#4173));
#1202=EDGE_LOOP('',(#4174,#4175,#4176,#4177,#4178,#4179,#4180,#4181,#4182));
#1203=EDGE_LOOP('',(#4183,#4184,#4185,#4186));
#1204=EDGE_LOOP('',(#4187,#4188,#4189,#4190));
#1205=EDGE_LOOP('',(#4191,#4192,#4193,#4194));
#1206=EDGE_LOOP('',(#4195,#4196,#4197,#4198));
#1207=EDGE_LOOP('',(#4199,#4200,#4201,#4202));
#1208=EDGE_LOOP('',(#4203,#4204,#4205,#4206));
#1209=EDGE_LOOP('',(#4207));
#1210=EDGE_LOOP('',(#4208,#4209,#4210,#4211,#4212,#4213));
#1211=EDGE_LOOP('',(#4214));
#1212=EDGE_LOOP('',(#4215,#4216,#4217,#4218));
#1213=EDGE_LOOP('',(#4219));
#1214=EDGE_LOOP('',(#4220,#4221,#4222,#4223));
#1215=EDGE_LOOP('',(#4224));
#1216=EDGE_LOOP('',(#4225,#4226,#4227,#4228));
#1217=EDGE_LOOP('',(#4229,#4230,#4231,#4232));
#1218=EDGE_LOOP('',(#4233,#4234,#4235,#4236));
#1219=EDGE_LOOP('',(#4237,#4238,#4239,#4240));
#1220=EDGE_LOOP('',(#4241,#4242,#4243,#4244));
#1221=EDGE_LOOP('',(#4245,#4246,#4247,#4248));
#1222=EDGE_LOOP('',(#4249,#4250,#4251,#4252,#4253,#4254));
#1223=EDGE_LOOP('',(#4255));
#1224=EDGE_LOOP('',(#4256));
#1225=EDGE_LOOP('',(#4257,#4258,#4259,#4260));
#1226=EDGE_LOOP('',(#4261,#4262,#4263,#4264));
#1227=EDGE_LOOP('',(#4265));
#1228=EDGE_LOOP('',(#4266));
#1229=EDGE_LOOP('',(#4267));
#1230=EDGE_LOOP('',(#4268));
#1231=EDGE_LOOP('',(#4269,#4270));
#1232=EDGE_LOOP('',(#4271));
#1233=EDGE_LOOP('',(#4272,#4273,#4274,#4275,#4276,#4277,#4278,#4279,#4280,
#4281));
#1234=EDGE_LOOP('',(#4282));
#1235=EDGE_LOOP('',(#4283));
#1236=EDGE_LOOP('',(#4284));
#1237=EDGE_LOOP('',(#4285));
#1238=EDGE_LOOP('',(#4286,#4287,#4288,#4289));
#1239=EDGE_LOOP('',(#4290,#4291,#4292,#4293));
#1240=EDGE_LOOP('',(#4294));
#1241=EDGE_LOOP('',(#4295));
#1242=EDGE_LOOP('',(#4296));
#1243=EDGE_LOOP('',(#4297));
#1244=EDGE_LOOP('',(#4298));
#1245=EDGE_LOOP('',(#4299,#4300,#4301,#4302));
#1246=EDGE_LOOP('',(#4303,#4304,#4305,#4306));
#1247=EDGE_LOOP('',(#4307,#4308,#4309,#4310));
#1248=EDGE_LOOP('',(#4311));
#1249=EDGE_LOOP('',(#4312,#4313,#4314,#4315));
#1250=EDGE_LOOP('',(#4316));
#1251=EDGE_LOOP('',(#4317,#4318,#4319,#4320));
#1252=EDGE_LOOP('',(#4321,#4322,#4323,#4324));
#1253=EDGE_LOOP('',(#4325,#4326,#4327,#4328));
#1254=EDGE_LOOP('',(#4329,#4330,#4331,#4332));
#1255=EDGE_LOOP('',(#4333,#4334,#4335,#4336));
#1256=EDGE_LOOP('',(#4337,#4338,#4339,#4340));
#1257=EDGE_LOOP('',(#4341,#4342,#4343,#4344,#4345,#4346));
#1258=EDGE_LOOP('',(#4347));
#1259=EDGE_LOOP('',(#4348));
#1260=EDGE_LOOP('',(#4349,#4350,#4351,#4352));
#1261=EDGE_LOOP('',(#4353,#4354,#4355,#4356));
#1262=EDGE_LOOP('',(#4357));
#1263=EDGE_LOOP('',(#4358));
#1264=EDGE_LOOP('',(#4359));
#1265=EDGE_LOOP('',(#4360));
#1266=EDGE_LOOP('',(#4361,#4362));
#1267=EDGE_LOOP('',(#4363));
#1268=EDGE_LOOP('',(#4364,#4365,#4366,#4367));
#1269=EDGE_LOOP('',(#4368));
#1270=EDGE_LOOP('',(#4369));
#1271=EDGE_LOOP('',(#4370));
#1272=EDGE_LOOP('',(#4371));
#1273=EDGE_LOOP('',(#4372));
#1274=EDGE_LOOP('',(#4373,#4374,#4375,#4376));
#1275=EDGE_LOOP('',(#4377,#4378,#4379,#4380,#4381,#4382,#4383,#4384,#4385,
#4386));
#1276=EDGE_LOOP('',(#4387));
#1277=EDGE_LOOP('',(#4388));
#1278=EDGE_LOOP('',(#4389));
#1279=EDGE_LOOP('',(#4390));
#1280=EDGE_LOOP('',(#4391,#4392,#4393,#4394));
#1281=EDGE_LOOP('',(#4395,#4396,#4397,#4398));
#1282=EDGE_LOOP('',(#4399,#4400,#4401,#4402));
#1283=EDGE_LOOP('',(#4403,#4404,#4405,#4406));
#1284=EDGE_LOOP('',(#4407,#4408,#4409,#4410));
#1285=EDGE_LOOP('',(#4411,#4412,#4413,#4414));
#1286=EDGE_LOOP('',(#4415,#4416,#4417,#4418));
#1287=EDGE_LOOP('',(#4419,#4420,#4421,#4422));
#1288=EDGE_LOOP('',(#4423,#4424,#4425,#4426));
#1289=EDGE_LOOP('',(#4427,#4428,#4429,#4430));
#1290=EDGE_LOOP('',(#4431,#4432,#4433,#4434,#4435,#4436,#4437,#4438,#4439,
#4440));
#1291=EDGE_LOOP('',(#4441));
#1292=EDGE_LOOP('',(#4442));
#1293=EDGE_LOOP('',(#4443));
#1294=EDGE_LOOP('',(#4444));
#1295=EDGE_LOOP('',(#4445,#4446,#4447,#4448));
#1296=EDGE_LOOP('',(#4449,#4450,#4451,#4452));
#1297=EDGE_LOOP('',(#4453,#4454,#4455,#4456));
#1298=EDGE_LOOP('',(#4457,#4458,#4459,#4460));
#1299=EDGE_LOOP('',(#4461,#4462,#4463,#4464));
#1300=EDGE_LOOP('',(#4465,#4466,#4467,#4468));
#1301=EDGE_LOOP('',(#4469,#4470,#4471,#4472,#4473,#4474,#4475,#4476,#4477,
#4478));
#1302=EDGE_LOOP('',(#4479));
#1303=EDGE_LOOP('',(#4480));
#1304=EDGE_LOOP('',(#4481));
#1305=EDGE_LOOP('',(#4482));
#1306=EDGE_LOOP('',(#4483));
#1307=EDGE_LOOP('',(#4484));
#1308=EDGE_LOOP('',(#4485,#4486,#4487,#4488));
#1309=EDGE_LOOP('',(#4489));
#1310=EDGE_LOOP('',(#4490));
#1311=EDGE_LOOP('',(#4491,#4492,#4493,#4494));
#1312=EDGE_LOOP('',(#4495,#4496,#4497,#4498));
#1313=EDGE_LOOP('',(#4499));
#1314=EDGE_LOOP('',(#4500));
#1315=EDGE_LOOP('',(#4501,#4502,#4503,#4504));
#1316=EDGE_LOOP('',(#4505,#4506,#4507,#4508));
#1317=EDGE_LOOP('',(#4509));
#1318=EDGE_LOOP('',(#4510));
#1319=EDGE_LOOP('',(#4511,#4512,#4513,#4514));
#1320=EDGE_LOOP('',(#4515,#4516,#4517,#4518));
#1321=EDGE_LOOP('',(#4519));
#1322=EDGE_LOOP('',(#4520));
#1323=EDGE_LOOP('',(#4521));
#1324=EDGE_LOOP('',(#4522));
#1325=EDGE_LOOP('',(#4523,#4524,#4525,#4526));
#1326=EDGE_LOOP('',(#4527));
#1327=EDGE_LOOP('',(#4528,#4529,#4530,#4531));
#1328=EDGE_LOOP('',(#4532));
#1329=EDGE_LOOP('',(#4533,#4534,#4535,#4536));
#1330=EDGE_LOOP('',(#4537,#4538,#4539,#4540));
#1331=EDGE_LOOP('',(#4541,#4542,#4543,#4544));
#1332=EDGE_LOOP('',(#4545,#4546,#4547,#4548));
#1333=EDGE_LOOP('',(#4549,#4550,#4551,#4552));
#1334=EDGE_LOOP('',(#4553,#4554,#4555,#4556));
#1335=EDGE_LOOP('',(#4557,#4558,#4559,#4560));
#1336=EDGE_LOOP('',(#4561,#4562,#4563,#4564));
#1337=EDGE_LOOP('',(#4565,#4566,#4567,#4568));
#1338=EDGE_LOOP('',(#4569,#4570,#4571,#4572));
#1339=EDGE_LOOP('',(#4573));
#1340=EDGE_LOOP('',(#4574));
#1341=EDGE_LOOP('',(#4575));
#1342=EDGE_LOOP('',(#4576));
#1343=EDGE_LOOP('',(#4577));
#1344=EDGE_LOOP('',(#4578));
#1345=EDGE_LOOP('',(#4579));
#1346=EDGE_LOOP('',(#4580,#4581,#4582,#4583));
#1347=EDGE_LOOP('',(#4584));
#1348=EDGE_LOOP('',(#4585));
#1349=EDGE_LOOP('',(#4586));
#1350=EDGE_LOOP('',(#4587));
#1351=EDGE_LOOP('',(#4588));
#1352=EDGE_LOOP('',(#4589));
#1353=EDGE_LOOP('',(#4590));
#1354=EDGE_LOOP('',(#4591,#4592,#4593,#4594));
#1355=EDGE_LOOP('',(#4595,#4596,#4597,#4598));
#1356=EDGE_LOOP('',(#4599));
#1357=EDGE_LOOP('',(#4600));
#1358=EDGE_LOOP('',(#4601));
#1359=EDGE_LOOP('',(#4602));
#1360=EDGE_LOOP('',(#4603,#4604,#4605,#4606));
#1361=EDGE_LOOP('',(#4607,#4608,#4609,#4610));
#1362=EDGE_LOOP('',(#4611,#4612,#4613,#4614));
#1363=EDGE_LOOP('',(#4615,#4616,#4617,#4618));
#1364=EDGE_LOOP('',(#4619,#4620,#4621,#4622));
#1365=EDGE_LOOP('',(#4623,#4624,#4625,#4626));
#1366=EDGE_LOOP('',(#4627,#4628,#4629,#4630,#4631,#4632));
#1367=EDGE_LOOP('',(#4633,#4634,#4635,#4636,#4637,#4638));
#1368=EDGE_LOOP('',(#4639));
#1369=EDGE_LOOP('',(#4640));
#1370=EDGE_LOOP('',(#4641,#4642,#4643,#4644));
#1371=EDGE_LOOP('',(#4645));
#1372=EDGE_LOOP('',(#4646));
#1373=EDGE_LOOP('',(#4647,#4648,#4649,#4650));
#1374=EDGE_LOOP('',(#4651,#4652,#4653,#4654));
#1375=EDGE_LOOP('',(#4655,#4656,#4657,#4658));
#1376=EDGE_LOOP('',(#4659));
#1377=EDGE_LOOP('',(#4660));
#1378=EDGE_LOOP('',(#4661,#4662,#4663,#4664));
#1379=EDGE_LOOP('',(#4665,#4666,#4667,#4668));
#1380=EDGE_LOOP('',(#4669,#4670,#4671,#4672));
#1381=EDGE_LOOP('',(#4673,#4674,#4675,#4676));
#1382=EDGE_LOOP('',(#4677));
#1383=EDGE_LOOP('',(#4678));
#1384=EDGE_LOOP('',(#4679,#4680,#4681,#4682));
#1385=EDGE_LOOP('',(#4683));
#1386=EDGE_LOOP('',(#4684));
#1387=EDGE_LOOP('',(#4685,#4686,#4687,#4688,#4689,#4690,#4691,#4692,#4693));
#1388=EDGE_LOOP('',(#4694,#4695,#4696,#4697,#4698,#4699,#4700,#4701,#4702));
#1389=EDGE_LOOP('',(#4703,#4704,#4705,#4706));
#1390=EDGE_LOOP('',(#4707,#4708,#4709,#4710));
#1391=EDGE_LOOP('',(#4711,#4712,#4713,#4714));
#1392=EDGE_LOOP('',(#4715,#4716,#4717,#4718));
#1393=EDGE_LOOP('',(#4719,#4720,#4721,#4722));
#1394=EDGE_LOOP('',(#4723,#4724,#4725,#4726));
#1395=EDGE_LOOP('',(#4727,#4728,#4729,#4730));
#1396=EDGE_LOOP('',(#4731));
#1397=EDGE_LOOP('',(#4732));
#1398=EDGE_LOOP('',(#4733));
#1399=EDGE_LOOP('',(#4734));
#1400=EDGE_LOOP('',(#4735,#4736,#4737,#4738,#4739,#4740));
#1401=EDGE_LOOP('',(#4741));
#1402=EDGE_LOOP('',(#4742,#4743,#4744,#4745,#4746,#4747));
#1403=EDGE_LOOP('',(#4748));
#1404=EDGE_LOOP('',(#4749,#4750,#4751,#4752));
#1405=EDGE_LOOP('',(#4753,#4754,#4755,#4756));
#1406=EDGE_LOOP('',(#4757,#4758,#4759,#4760));
#1407=EDGE_LOOP('',(#4761,#4762,#4763,#4764));
#1408=EDGE_LOOP('',(#4765,#4766,#4767,#4768));
#1409=EDGE_LOOP('',(#4769,#4770,#4771,#4772));
#1410=EDGE_LOOP('',(#4773,#4774,#4775,#4776));
#1411=EDGE_LOOP('',(#4777));
#1412=EDGE_LOOP('',(#4778));
#1413=EDGE_LOOP('',(#4779,#4780,#4781,#4782));
#1414=EDGE_LOOP('',(#4783,#4784,#4785,#4786));
#1415=EDGE_LOOP('',(#4787,#4788,#4789,#4790));
#1416=EDGE_LOOP('',(#4791));
#1417=EDGE_LOOP('',(#4792));
#1418=EDGE_LOOP('',(#4793,#4794,#4795,#4796));
#1419=EDGE_LOOP('',(#4797,#4798,#4799,#4800));
#1420=EDGE_LOOP('',(#4801,#4802,#4803,#4804));
#1421=EDGE_LOOP('',(#4805));
#1422=EDGE_LOOP('',(#4806));
#1423=EDGE_LOOP('',(#4807));
#1424=EDGE_LOOP('',(#4808));
#1425=EDGE_LOOP('',(#4809));
#1426=EDGE_LOOP('',(#4810,#4811,#4812,#4813));
#1427=EDGE_LOOP('',(#4814,#4815,#4816,#4817));
#1428=EDGE_LOOP('',(#4818,#4819,#4820,#4821));
#1429=EDGE_LOOP('',(#4822));
#1430=EDGE_LOOP('',(#4823));
#1431=EDGE_LOOP('',(#4824,#4825,#4826,#4827));
#1432=EDGE_LOOP('',(#4828,#4829,#4830,#4831));
#1433=EDGE_LOOP('',(#4832,#4833,#4834,#4835));
#1434=EDGE_LOOP('',(#4836));
#1435=EDGE_LOOP('',(#4837,#4838,#4839,#4840));
#1436=EDGE_LOOP('',(#4841,#4842,#4843,#4844));
#1437=EDGE_LOOP('',(#4845,#4846,#4847,#4848));
#1438=EDGE_LOOP('',(#4849,#4850,#4851,#4852));
#1439=EDGE_LOOP('',(#4853,#4854,#4855,#4856));
#1440=EDGE_LOOP('',(#4857,#4858,#4859,#4860));
#1441=EDGE_LOOP('',(#4861,#4862,#4863,#4864,#4865,#4866));
#1442=EDGE_LOOP('',(#4867,#4868,#4869,#4870,#4871,#4872));
#1443=EDGE_LOOP('',(#4873,#4874,#4875,#4876));
#1444=EDGE_LOOP('',(#4877));
#1445=EDGE_LOOP('',(#4878));
#1446=EDGE_LOOP('',(#4879,#4880,#4881,#4882));
#1447=EDGE_LOOP('',(#4883,#4884,#4885,#4886,#4887));
#1448=EDGE_LOOP('',(#4888,#4889,#4890,#4891));
#1449=EDGE_LOOP('',(#4892,#4893,#4894,#4895));
#1450=EDGE_LOOP('',(#4896,#4897,#4898,#4899));
#1451=EDGE_LOOP('',(#4900,#4901,#4902,#4903));
#1452=EDGE_LOOP('',(#4904,#4905,#4906,#4907,#4908,#4909,#4910));
#1453=EDGE_LOOP('',(#4911));
#1454=EDGE_LOOP('',(#4912));
#1455=EDGE_LOOP('',(#4913,#4914,#4915,#4916));
#1456=EDGE_LOOP('',(#4917));
#1457=EDGE_LOOP('',(#4918,#4919,#4920));
#1458=EDGE_LOOP('',(#4921,#4922,#4923));
#1459=EDGE_LOOP('',(#4924,#4925,#4926));
#1460=EDGE_LOOP('',(#4927,#4928,#4929));
#1461=EDGE_LOOP('',(#4930,#4931,#4932,#4933,#4934,#4935));
#1462=EDGE_LOOP('',(#4936,#4937,#4938,#4939,#4940,#4941));
#1463=EDGE_LOOP('',(#4942,#4943,#4944,#4945,#4946,#4947));
#1464=EDGE_LOOP('',(#4948,#4949,#4950,#4951,#4952,#4953));
#1465=EDGE_LOOP('',(#4954,#4955,#4956,#4957));
#1466=EDGE_LOOP('',(#4958));
#1467=EDGE_LOOP('',(#4959,#4960));
#1468=EDGE_LOOP('',(#4961,#4962,#4963));
#1469=EDGE_LOOP('',(#4964,#4965));
#1470=EDGE_LOOP('',(#4966,#4967));
#1471=EDGE_LOOP('',(#4968,#4969,#4970,#4971));
#1472=EDGE_LOOP('',(#4972,#4973,#4974,#4975));
#1473=EDGE_LOOP('',(#4976,#4977,#4978,#4979));
#1474=EDGE_LOOP('',(#4980,#4981,#4982,#4983));
#1475=EDGE_LOOP('',(#4984,#4985,#4986,#4987));
#1476=EDGE_LOOP('',(#4988,#4989,#4990,#4991,#4992,#4993,#4994,#4995,#4996,
#4997,#4998,#4999));
#1477=EDGE_LOOP('',(#5000));
#1478=EDGE_LOOP('',(#5001,#5002,#5003,#5004));
#1479=EDGE_LOOP('',(#5005,#5006,#5007,#5008));
#1480=EDGE_LOOP('',(#5009,#5010,#5011,#5012));
#1481=EDGE_LOOP('',(#5013,#5014,#5015,#5016));
#1482=EDGE_LOOP('',(#5017,#5018,#5019,#5020));
#1483=EDGE_LOOP('',(#5021,#5022,#5023,#5024));
#1484=EDGE_LOOP('',(#5025,#5026,#5027,#5028));
#1485=EDGE_LOOP('',(#5029,#5030,#5031,#5032));
#1486=EDGE_LOOP('',(#5033,#5034,#5035,#5036));
#1487=EDGE_LOOP('',(#5037,#5038,#5039,#5040));
#1488=EDGE_LOOP('',(#5041,#5042,#5043,#5044));
#1489=EDGE_LOOP('',(#5045,#5046,#5047,#5048));
#1490=EDGE_LOOP('',(#5049,#5050,#5051,#5052));
#1491=EDGE_LOOP('',(#5053,#5054,#5055,#5056));
#1492=EDGE_LOOP('',(#5057,#5058,#5059,#5060));
#1493=EDGE_LOOP('',(#5061));
#1494=EDGE_LOOP('',(#5062));
#1495=EDGE_LOOP('',(#5063));
#1496=EDGE_LOOP('',(#5064));
#1497=EDGE_LOOP('',(#5065,#5066,#5067,#5068));
#1498=EDGE_LOOP('',(#5069,#5070,#5071,#5072));
#1499=EDGE_LOOP('',(#5073,#5074,#5075,#5076));
#1500=EDGE_LOOP('',(#5077,#5078,#5079,#5080));
#1501=EDGE_LOOP('',(#5081,#5082,#5083,#5084));
#1502=EDGE_LOOP('',(#5085,#5086,#5087,#5088));
#1503=EDGE_LOOP('',(#5089,#5090,#5091,#5092));
#1504=EDGE_LOOP('',(#5093,#5094,#5095,#5096));
#1505=EDGE_LOOP('',(#5097,#5098,#5099,#5100));
#1506=EDGE_LOOP('',(#5101,#5102,#5103,#5104));
#1507=EDGE_LOOP('',(#5105,#5106,#5107,#5108));
#1508=EDGE_LOOP('',(#5109,#5110,#5111,#5112));
#1509=EDGE_LOOP('',(#5113,#5114,#5115,#5116,#5117,#5118));
#1510=EDGE_LOOP('',(#5119,#5120,#5121,#5122,#5123,#5124));
#1511=EDGE_LOOP('',(#5125));
#1512=EDGE_LOOP('',(#5126));
#1513=EDGE_LOOP('',(#5127,#5128,#5129,#5130));
#1514=EDGE_LOOP('',(#5131,#5132,#5133,#5134));
#1515=EDGE_LOOP('',(#5135,#5136,#5137,#5138));
#1516=EDGE_LOOP('',(#5139));
#1517=EDGE_LOOP('',(#5140));
#1518=EDGE_LOOP('',(#5141,#5142,#5143,#5144));
#1519=EDGE_LOOP('',(#5145,#5146,#5147,#5148));
#1520=LINE('',#8342,#1938);
#1521=LINE('',#8349,#1939);
#1522=LINE('',#8356,#1940);
#1523=LINE('',#8365,#1941);
#1524=LINE('',#8373,#1942);
#1525=LINE('',#8399,#1943);
#1526=LINE('',#8402,#1944);
#1527=LINE('',#8406,#1945);
#1528=LINE('',#8426,#1946);
#1529=LINE('',#8432,#1947);
#1530=LINE('',#8437,#1948);
#1531=LINE('',#8454,#1949);
#1532=LINE('',#8457,#1950);
#1533=LINE('',#8461,#1951);
#1534=LINE('',#8481,#1952);
#1535=LINE('',#8487,#1953);
#1536=LINE('',#8492,#1954);
#1537=LINE('',#8509,#1955);
#1538=LINE('',#8512,#1956);
#1539=LINE('',#8516,#1957);
#1540=LINE('',#8536,#1958);
#1541=LINE('',#8542,#1959);
#1542=LINE('',#8547,#1960);
#1543=LINE('',#8564,#1961);
#1544=LINE('',#8566,#1962);
#1545=LINE('',#8568,#1963);
#1546=LINE('',#8587,#1964);
#1547=LINE('',#8589,#1965);
#1548=LINE('',#8605,#1966);
#1549=LINE('',#8606,#1967);
#1550=LINE('',#8610,#1968);
#1551=LINE('',#8615,#1969);
#1552=LINE('',#8620,#1970);
#1553=LINE('',#8627,#1971);
#1554=LINE('',#8645,#1972);
#1555=LINE('',#8663,#1973);
#1556=LINE('',#8681,#1974);
#1557=LINE('',#8687,#1975);
#1558=LINE('',#8689,#1976);
#1559=LINE('',#8691,#1977);
#1560=LINE('',#8692,#1978);
#1561=LINE('',#8695,#1979);
#1562=LINE('',#8697,#1980);
#1563=LINE('',#8698,#1981);
#1564=LINE('',#8701,#1982);
#1565=LINE('',#8703,#1983);
#1566=LINE('',#8704,#1984);
#1567=LINE('',#8706,#1985);
#1568=LINE('',#8707,#1986);
#1569=LINE('',#8714,#1987);
#1570=LINE('',#8716,#1988);
#1571=LINE('',#8718,#1989);
#1572=LINE('',#8720,#1990);
#1573=LINE('',#8722,#1991);
#1574=LINE('',#8723,#1992);
#1575=LINE('',#8729,#1993);
#1576=LINE('',#8730,#1994);
#1577=LINE('',#8731,#1995);
#1578=LINE('',#8734,#1996);
#1579=LINE('',#8735,#1997);
#1580=LINE('',#8738,#1998);
#1581=LINE('',#8739,#1999);
#1582=LINE('',#8742,#2000);
#1583=LINE('',#8743,#2001);
#1584=LINE('',#8746,#2002);
#1585=LINE('',#8747,#2003);
#1586=LINE('',#8749,#2004);
#1587=LINE('',#8754,#2005);
#1588=LINE('',#8761,#2006);
#1589=LINE('',#8769,#2007);
#1590=LINE('',#8774,#2008);
#1591=LINE('',#8782,#2009);
#1592=LINE('',#8787,#2010);
#1593=LINE('',#8794,#2011);
#1594=LINE('',#8799,#2012);
#1595=LINE('',#8801,#2013);
#1596=LINE('',#8803,#2014);
#1597=LINE('',#8804,#2015);
#1598=LINE('',#8807,#2016);
#1599=LINE('',#8809,#2017);
#1600=LINE('',#8810,#2018);
#1601=LINE('',#8813,#2019);
#1602=LINE('',#8815,#2020);
#1603=LINE('',#8816,#2021);
#1604=LINE('',#8818,#2022);
#1605=LINE('',#8819,#2023);
#1606=LINE('',#8827,#2024);
#1607=LINE('',#8835,#2025);
#1608=LINE('',#8840,#2026);
#1609=LINE('',#8848,#2027);
#1610=LINE('',#8853,#2028);
#1611=LINE('',#8860,#2029);
#1612=LINE('',#8865,#2030);
#1613=LINE('',#8867,#2031);
#1614=LINE('',#8869,#2032);
#1615=LINE('',#8870,#2033);
#1616=LINE('',#8873,#2034);
#1617=LINE('',#8875,#2035);
#1618=LINE('',#8876,#2036);
#1619=LINE('',#8879,#2037);
#1620=LINE('',#8881,#2038);
#1621=LINE('',#8882,#2039);
#1622=LINE('',#8884,#2040);
#1623=LINE('',#8885,#2041);
#1624=LINE('',#8893,#2042);
#1625=LINE('',#8898,#2043);
#1626=LINE('',#8904,#2044);
#1627=LINE('',#8930,#2045);
#1628=LINE('',#8932,#2046);
#1629=LINE('',#8933,#2047);
#1630=LINE('',#8936,#2048);
#1631=LINE('',#8937,#2049);
#1632=LINE('',#8940,#2050);
#1633=LINE('',#8941,#2051);
#1634=LINE('',#8944,#2052);
#1635=LINE('',#8945,#2053);
#1636=LINE('',#8948,#2054);
#1637=LINE('',#8949,#2055);
#1638=LINE('',#8951,#2056);
#1639=LINE('',#8960,#2057);
#1640=LINE('',#8967,#2058);
#1641=LINE('',#8974,#2059);
#1642=LINE('',#8980,#2060);
#1643=LINE('',#8986,#2061);
#1644=LINE('',#8992,#2062);
#1645=LINE('',#8997,#2063);
#1646=LINE('',#9001,#2064);
#1647=LINE('',#9005,#2065);
#1648=LINE('',#9008,#2066);
#1649=LINE('',#9011,#2067);
#1650=LINE('',#9013,#2068);
#1651=LINE('',#9015,#2069);
#1652=LINE('',#9017,#2070);
#1653=LINE('',#9018,#2071);
#1654=LINE('',#9023,#2072);
#1655=LINE('',#9029,#2073);
#1656=LINE('',#9039,#2074);
#1657=LINE('',#9041,#2075);
#1658=LINE('',#9042,#2076);
#1659=LINE('',#9045,#2077);
#1660=LINE('',#9046,#2078);
#1661=LINE('',#9049,#2079);
#1662=LINE('',#9050,#2080);
#1663=LINE('',#9052,#2081);
#1664=LINE('',#9059,#2082);
#1665=LINE('',#9066,#2083);
#1666=LINE('',#9073,#2084);
#1667=LINE('',#9079,#2085);
#1668=LINE('',#9085,#2086);
#1669=LINE('',#9091,#2087);
#1670=LINE('',#9096,#2088);
#1671=LINE('',#9100,#2089);
#1672=LINE('',#9104,#2090);
#1673=LINE('',#9107,#2091);
#1674=LINE('',#9110,#2092);
#1675=LINE('',#9112,#2093);
#1676=LINE('',#9114,#2094);
#1677=LINE('',#9116,#2095);
#1678=LINE('',#9117,#2096);
#1679=LINE('',#9122,#2097);
#1680=LINE('',#9128,#2098);
#1681=LINE('',#9139,#2099);
#1682=LINE('',#9140,#2100);
#1683=LINE('',#9141,#2101);
#1684=LINE('',#9144,#2102);
#1685=LINE('',#9145,#2103);
#1686=LINE('',#9148,#2104);
#1687=LINE('',#9149,#2105);
#1688=LINE('',#9151,#2106);
#1689=LINE('',#9158,#2107);
#1690=LINE('',#9164,#2108);
#1691=LINE('',#9170,#2109);
#1692=LINE('',#9176,#2110);
#1693=LINE('',#9181,#2111);
#1694=LINE('',#9183,#2112);
#1695=LINE('',#9185,#2113);
#1696=LINE('',#9186,#2114);
#1697=LINE('',#9190,#2115);
#1698=LINE('',#9192,#2116);
#1699=LINE('',#9194,#2117);
#1700=LINE('',#9195,#2118);
#1701=LINE('',#9198,#2119);
#1702=LINE('',#9200,#2120);
#1703=LINE('',#9201,#2121);
#1704=LINE('',#9204,#2122);
#1705=LINE('',#9206,#2123);
#1706=LINE('',#9207,#2124);
#1707=LINE('',#9211,#2125);
#1708=LINE('',#9213,#2126);
#1709=LINE('',#9215,#2127);
#1710=LINE('',#9217,#2128);
#1711=LINE('',#9218,#2129);
#1712=LINE('',#9221,#2130);
#1713=LINE('',#9222,#2131);
#1714=LINE('',#9225,#2132);
#1715=LINE('',#9226,#2133);
#1716=LINE('',#9231,#2134);
#1717=LINE('',#9232,#2135);
#1718=LINE('',#9235,#2136);
#1719=LINE('',#9236,#2137);
#1720=LINE('',#9238,#2138);
#1721=LINE('',#9249,#2139);
#1722=LINE('',#9255,#2140);
#1723=LINE('',#9259,#2141);
#1724=LINE('',#9272,#2142);
#1725=LINE('',#9280,#2143);
#1726=LINE('',#9285,#2144);
#1727=LINE('',#9294,#2145);
#1728=LINE('',#9301,#2146);
#1729=LINE('',#9308,#2147);
#1730=LINE('',#9314,#2148);
#1731=LINE('',#9320,#2149);
#1732=LINE('',#9326,#2150);
#1733=LINE('',#9332,#2151);
#1734=LINE('',#9337,#2152);
#1735=LINE('',#9339,#2153);
#1736=LINE('',#9341,#2154);
#1737=LINE('',#9342,#2155);
#1738=LINE('',#9345,#2156);
#1739=LINE('',#9347,#2157);
#1740=LINE('',#9348,#2158);
#1741=LINE('',#9351,#2159);
#1742=LINE('',#9353,#2160);
#1743=LINE('',#9354,#2161);
#1744=LINE('',#9356,#2162);
#1745=LINE('',#9357,#2163);
#1746=LINE('',#9368,#2164);
#1747=LINE('',#9374,#2165);
#1748=LINE('',#9382,#2166);
#1749=LINE('',#9384,#2167);
#1750=LINE('',#9386,#2168);
#1751=LINE('',#9387,#2169);
#1752=LINE('',#9390,#2170);
#1753=LINE('',#9392,#2171);
#1754=LINE('',#9393,#2172);
#1755=LINE('',#9396,#2173);
#1756=LINE('',#9398,#2174);
#1757=LINE('',#9399,#2175);
#1758=LINE('',#9402,#2176);
#1759=LINE('',#9404,#2177);
#1760=LINE('',#9405,#2178);
#1761=LINE('',#9408,#2179);
#1762=LINE('',#9410,#2180);
#1763=LINE('',#9411,#2181);
#1764=LINE('',#9413,#2182);
#1765=LINE('',#9414,#2183);
#1766=LINE('',#9424,#2184);
#1767=LINE('',#9433,#2185);
#1768=LINE('',#9437,#2186);
#1769=LINE('',#9441,#2187);
#1770=LINE('',#9448,#2188);
#1771=LINE('',#9450,#2189);
#1772=LINE('',#9456,#2190);
#1773=LINE('',#9460,#2191);
#1774=LINE('',#9467,#2192);
#1775=LINE('',#9482,#2193);
#1776=LINE('',#9503,#2194);
#1777=LINE('',#9528,#2195);
#1778=LINE('',#9529,#2196);
#1779=LINE('',#9531,#2197);
#1780=LINE('',#9533,#2198);
#1781=LINE('',#9538,#2199);
#1782=LINE('',#9541,#2200);
#1783=LINE('',#9543,#2201);
#1784=LINE('',#9551,#2202);
#1785=LINE('',#9553,#2203);
#1786=LINE('',#9555,#2204);
#1787=LINE('',#9557,#2205);
#1788=LINE('',#9559,#2206);
#1789=LINE('',#9560,#2207);
#1790=LINE('',#9566,#2208);
#1791=LINE('',#9568,#2209);
#1792=LINE('',#9570,#2210);
#1793=LINE('',#9572,#2211);
#1794=LINE('',#9574,#2212);
#1795=LINE('',#9575,#2213);
#1796=LINE('',#9579,#2214);
#1797=LINE('',#9580,#2215);
#1798=LINE('',#9582,#2216);
#1799=LINE('',#9584,#2217);
#1800=LINE('',#9586,#2218);
#1801=LINE('',#9588,#2219);
#1802=LINE('',#9592,#2220);
#1803=LINE('',#9600,#2221);
#1804=LINE('',#9604,#2222);
#1805=LINE('',#9608,#2223);
#1806=LINE('',#9613,#2224);
#1807=LINE('',#9619,#2225);
#1808=LINE('',#9625,#2226);
#1809=LINE('',#9636,#2227);
#1810=LINE('',#9640,#2228);
#1811=LINE('',#9644,#2229);
#1812=LINE('',#9651,#2230);
#1813=LINE('',#9655,#2231);
#1814=LINE('',#9659,#2232);
#1815=LINE('',#9664,#2233);
#1816=LINE('',#9666,#2234);
#1817=LINE('',#9668,#2235);
#1818=LINE('',#9669,#2236);
#1819=LINE('',#9672,#2237);
#1820=LINE('',#9674,#2238);
#1821=LINE('',#9675,#2239);
#1822=LINE('',#9678,#2240);
#1823=LINE('',#9680,#2241);
#1824=LINE('',#9681,#2242);
#1825=LINE('',#9684,#2243);
#1826=LINE('',#9686,#2244);
#1827=LINE('',#9687,#2245);
#1828=LINE('',#9690,#2246);
#1829=LINE('',#9692,#2247);
#1830=LINE('',#9693,#2248);
#1831=LINE('',#9695,#2249);
#1832=LINE('',#9696,#2250);
#1833=LINE('',#9704,#2251);
#1834=LINE('',#9715,#2252);
#1835=LINE('',#9717,#2253);
#1836=LINE('',#9718,#2254);
#1837=LINE('',#9723,#2255);
#1838=LINE('',#9725,#2256);
#1839=LINE('',#9731,#2257);
#1840=LINE('',#9732,#2258);
#1841=LINE('',#9735,#2259);
#1842=LINE('',#9741,#2260);
#1843=LINE('',#9751,#2261);
#1844=LINE('',#9759,#2262);
#1845=LINE('',#9760,#2263);
#1846=LINE('',#9766,#2264);
#1847=LINE('',#9767,#2265);
#1848=LINE('',#9773,#2266);
#1849=LINE('',#9774,#2267);
#1850=LINE('',#9780,#2268);
#1851=LINE('',#9781,#2269);
#1852=LINE('',#9783,#2270);
#1853=LINE('',#9785,#2271);
#1854=LINE('',#9787,#2272);
#1855=LINE('',#9788,#2273);
#1856=LINE('',#9790,#2274);
#1857=LINE('',#9792,#2275);
#1858=LINE('',#9793,#2276);
#1859=LINE('',#9795,#2277);
#1860=LINE('',#9797,#2278);
#1861=LINE('',#9798,#2279);
#1862=LINE('',#9800,#2280);
#1863=LINE('',#9801,#2281);
#1864=LINE('',#9816,#2282);
#1865=LINE('',#9818,#2283);
#1866=LINE('',#9820,#2284);
#1867=LINE('',#9821,#2285);
#1868=LINE('',#9824,#2286);
#1869=LINE('',#9826,#2287);
#1870=LINE('',#9827,#2288);
#1871=LINE('',#9830,#2289);
#1872=LINE('',#9832,#2290);
#1873=LINE('',#9833,#2291);
#1874=LINE('',#9835,#2292);
#1875=LINE('',#9836,#2293);
#1876=LINE('',#9840,#2294);
#1877=LINE('',#9847,#2295);
#1878=LINE('',#9849,#2296);
#1879=LINE('',#9851,#2297);
#1880=LINE('',#9852,#2298);
#1881=LINE('',#9855,#2299);
#1882=LINE('',#9857,#2300);
#1883=LINE('',#9858,#2301);
#1884=LINE('',#9861,#2302);
#1885=LINE('',#9863,#2303);
#1886=LINE('',#9864,#2304);
#1887=LINE('',#9866,#2305);
#1888=LINE('',#9867,#2306);
#1889=LINE('',#9871,#2307);
#1890=LINE('',#9873,#2308);
#1891=LINE('',#9875,#2309);
#1892=LINE('',#9876,#2310);
#1893=LINE('',#9879,#2311);
#1894=LINE('',#9881,#2312);
#1895=LINE('',#9882,#2313);
#1896=LINE('',#9885,#2314);
#1897=LINE('',#9887,#2315);
#1898=LINE('',#9888,#2316);
#1899=LINE('',#9890,#2317);
#1900=LINE('',#9891,#2318);
#1901=LINE('',#9899,#2319);
#1902=LINE('',#9905,#2320);
#1903=LINE('',#9913,#2321);
#1904=LINE('',#9915,#2322);
#1905=LINE('',#9917,#2323);
#1906=LINE('',#9918,#2324);
#1907=LINE('',#9921,#2325);
#1908=LINE('',#9923,#2326);
#1909=LINE('',#9924,#2327);
#1910=LINE('',#9927,#2328);
#1911=LINE('',#9929,#2329);
#1912=LINE('',#9930,#2330);
#1913=LINE('',#9932,#2331);
#1914=LINE('',#9933,#2332);
#1915=LINE('',#9940,#2333);
#1916=LINE('',#9942,#2334);
#1917=LINE('',#9944,#2335);
#1918=LINE('',#9945,#2336);
#1919=LINE('',#9948,#2337);
#1920=LINE('',#9950,#2338);
#1921=LINE('',#9951,#2339);
#1922=LINE('',#9954,#2340);
#1923=LINE('',#9956,#2341);
#1924=LINE('',#9957,#2342);
#1925=LINE('',#9960,#2343);
#1926=LINE('',#9962,#2344);
#1927=LINE('',#9963,#2345);
#1928=LINE('',#9966,#2346);
#1929=LINE('',#9968,#2347);
#1930=LINE('',#9969,#2348);
#1931=LINE('',#9971,#2349);
#1932=LINE('',#9972,#2350);
#1933=LINE('',#9984,#2351);
#1934=LINE('',#9988,#2352);
#1935=LINE('',#9992,#2353);
#1936=LINE('',#9999,#2354);
#1937=LINE('',#10001,#2355);
#1938=VECTOR('',#6579,0.25);
#1939=VECTOR('',#6588,0.25);
#1940=VECTOR('',#6597,0.93);
#1941=VECTOR('',#6608,0.93);
#1942=VECTOR('',#6617,1.);
#1943=VECTOR('',#6652,1.);
#1944=VECTOR('',#6655,0.79);
#1945=VECTOR('',#6658,1.);
#1946=VECTOR('',#6659,1.);
#1947=VECTOR('',#6664,1.);
#1948=VECTOR('',#6669,1.);
#1949=VECTOR('',#6670,1.);
#1950=VECTOR('',#6673,0.79);
#1951=VECTOR('',#6676,1.);
#1952=VECTOR('',#6677,1.);
#1953=VECTOR('',#6682,1.);
#1954=VECTOR('',#6687,1.);
#1955=VECTOR('',#6688,1.);
#1956=VECTOR('',#6691,0.79);
#1957=VECTOR('',#6694,1.);
#1958=VECTOR('',#6695,1.);
#1959=VECTOR('',#6700,1.);
#1960=VECTOR('',#6705,1.);
#1961=VECTOR('',#6706,1.);
#1962=VECTOR('',#6709,0.79);
#1963=VECTOR('',#6710,1.);
#1964=VECTOR('',#6711,1.);
#1965=VECTOR('',#6712,1.);
#1966=VECTOR('',#6713,1.);
#1967=VECTOR('',#6714,0.79);
#1968=VECTOR('',#6717,1.);
#1969=VECTOR('',#6722,1.);
#1970=VECTOR('',#6727,1.);
#1971=VECTOR('',#6738,0.93);
#1972=VECTOR('',#6771,0.93);
#1973=VECTOR('',#6804,0.93);
#1974=VECTOR('',#6837,0.93);
#1975=VECTOR('',#6844,1.);
#1976=VECTOR('',#6845,1.);
#1977=VECTOR('',#6846,1.);
#1978=VECTOR('',#6847,1.);
#1979=VECTOR('',#6850,1.);
#1980=VECTOR('',#6851,1.);
#1981=VECTOR('',#6852,1.);
#1982=VECTOR('',#6855,1.);
#1983=VECTOR('',#6856,1.);
#1984=VECTOR('',#6857,1.);
#1985=VECTOR('',#6860,1.);
#1986=VECTOR('',#6861,1.);
#1987=VECTOR('',#6870,1.);
#1988=VECTOR('',#6871,1.);
#1989=VECTOR('',#6872,1.);
#1990=VECTOR('',#6873,1.);
#1991=VECTOR('',#6874,1.);
#1992=VECTOR('',#6875,1.);
#1993=VECTOR('',#6880,1.);
#1994=VECTOR('',#6881,1.);
#1995=VECTOR('',#6882,1.);
#1996=VECTOR('',#6885,1.);
#1997=VECTOR('',#6886,1.);
#1998=VECTOR('',#6889,1.);
#1999=VECTOR('',#6890,1.);
#2000=VECTOR('',#6893,1.);
#2001=VECTOR('',#6894,1.);
#2002=VECTOR('',#6897,1.);
#2003=VECTOR('',#6898,1.);
#2004=VECTOR('',#6901,1.);
#2005=VECTOR('',#6908,0.93);
#2006=VECTOR('',#6917,0.55);
#2007=VECTOR('',#6928,0.33);
#2008=VECTOR('',#6933,0.55);
#2009=VECTOR('',#6944,0.33);
#2010=VECTOR('',#6949,0.6);
#2011=VECTOR('',#6958,0.33);
#2012=VECTOR('',#6963,1.);
#2013=VECTOR('',#6964,1.);
#2014=VECTOR('',#6965,1.);
#2015=VECTOR('',#6966,1.);
#2016=VECTOR('',#6969,1.);
#2017=VECTOR('',#6970,1.);
#2018=VECTOR('',#6971,1.);
#2019=VECTOR('',#6974,1.);
#2020=VECTOR('',#6975,1.);
#2021=VECTOR('',#6976,1.);
#2022=VECTOR('',#6979,1.);
#2023=VECTOR('',#6980,1.);
#2024=VECTOR('',#6991,0.549999999999997);
#2025=VECTOR('',#7002,0.329999999999998);
#2026=VECTOR('',#7007,0.549999999999997);
#2027=VECTOR('',#7018,0.329999999999998);
#2028=VECTOR('',#7023,0.600000000000001);
#2029=VECTOR('',#7032,0.329999999999998);
#2030=VECTOR('',#7037,1.);
#2031=VECTOR('',#7038,1.);
#2032=VECTOR('',#7039,1.);
#2033=VECTOR('',#7040,1.);
#2034=VECTOR('',#7043,1.);
#2035=VECTOR('',#7044,1.);
#2036=VECTOR('',#7045,1.);
#2037=VECTOR('',#7048,1.);
#2038=VECTOR('',#7049,1.);
#2039=VECTOR('',#7050,1.);
#2040=VECTOR('',#7053,1.);
#2041=VECTOR('',#7054,1.);
#2042=VECTOR('',#7065,0.3);
#2043=VECTOR('',#7072,0.27);
#2044=VECTOR('',#7079,0.576175134594813);
#2045=VECTOR('',#7082,1.);
#2046=VECTOR('',#7083,1.);
#2047=VECTOR('',#7084,1.);
#2048=VECTOR('',#7087,1.);
#2049=VECTOR('',#7088,1.);
#2050=VECTOR('',#7091,1.);
#2051=VECTOR('',#7092,1.);
#2052=VECTOR('',#7095,1.);
#2053=VECTOR('',#7096,1.);
#2054=VECTOR('',#7099,1.);
#2055=VECTOR('',#7100,1.);
#2056=VECTOR('',#7103,1.);
#2057=VECTOR('',#7116,0.165);
#2058=VECTOR('',#7125,0.165);
#2059=VECTOR('',#7134,0.275);
#2060=VECTOR('',#7141,0.275);
#2061=VECTOR('',#7148,0.275);
#2062=VECTOR('',#7155,0.275);
#2063=VECTOR('',#7160,1.);
#2064=VECTOR('',#7163,1.);
#2065=VECTOR('',#7168,1.);
#2066=VECTOR('',#7171,1.);
#2067=VECTOR('',#7174,1.);
#2068=VECTOR('',#7175,1.);
#2069=VECTOR('',#7176,1.);
#2070=VECTOR('',#7177,1.);
#2071=VECTOR('',#7178,1.);
#2072=VECTOR('',#7183,0.93);
#2073=VECTOR('',#7190,1.3);
#2074=VECTOR('',#7205,1.);
#2075=VECTOR('',#7206,1.);
#2076=VECTOR('',#7207,1.);
#2077=VECTOR('',#7210,1.);
#2078=VECTOR('',#7211,1.);
#2079=VECTOR('',#7214,1.);
#2080=VECTOR('',#7215,1.);
#2081=VECTOR('',#7218,1.);
#2082=VECTOR('',#7227,0.165);
#2083=VECTOR('',#7236,0.165);
#2084=VECTOR('',#7245,0.275);
#2085=VECTOR('',#7252,0.275);
#2086=VECTOR('',#7259,0.275);
#2087=VECTOR('',#7266,0.275);
#2088=VECTOR('',#7271,1.);
#2089=VECTOR('',#7274,1.);
#2090=VECTOR('',#7279,1.);
#2091=VECTOR('',#7282,1.);
#2092=VECTOR('',#7285,1.);
#2093=VECTOR('',#7286,1.);
#2094=VECTOR('',#7287,1.);
#2095=VECTOR('',#7288,1.);
#2096=VECTOR('',#7289,1.);
#2097=VECTOR('',#7294,0.93);
#2098=VECTOR('',#7301,1.3);
#2099=VECTOR('',#7316,1.);
#2100=VECTOR('',#7317,1.);
#2101=VECTOR('',#7318,1.);
#2102=VECTOR('',#7321,1.);
#2103=VECTOR('',#7322,1.);
#2104=VECTOR('',#7325,1.);
#2105=VECTOR('',#7326,1.);
#2106=VECTOR('',#7329,1.);
#2107=VECTOR('',#7338,0.275);
#2108=VECTOR('',#7345,0.275);
#2109=VECTOR('',#7352,0.275);
#2110=VECTOR('',#7359,0.275);
#2111=VECTOR('',#7364,1.);
#2112=VECTOR('',#7365,1.);
#2113=VECTOR('',#7366,1.);
#2114=VECTOR('',#7367,1.);
#2115=VECTOR('',#7370,1.);
#2116=VECTOR('',#7371,1.);
#2117=VECTOR('',#7372,1.);
#2118=VECTOR('',#7373,1.);
#2119=VECTOR('',#7376,1.);
#2120=VECTOR('',#7377,1.);
#2121=VECTOR('',#7378,1.);
#2122=VECTOR('',#7381,1.);
#2123=VECTOR('',#7382,1.);
#2124=VECTOR('',#7383,1.);
#2125=VECTOR('',#7388,1.);
#2126=VECTOR('',#7389,1.);
#2127=VECTOR('',#7390,1.);
#2128=VECTOR('',#7391,1.);
#2129=VECTOR('',#7392,1.);
#2130=VECTOR('',#7395,1.);
#2131=VECTOR('',#7396,1.);
#2132=VECTOR('',#7399,1.);
#2133=VECTOR('',#7400,1.);
#2134=VECTOR('',#7407,1.);
#2135=VECTOR('',#7408,1.);
#2136=VECTOR('',#7411,1.);
#2137=VECTOR('',#7412,1.);
#2138=VECTOR('',#7415,1.);
#2139=VECTOR('',#7430,1.2);
#2140=VECTOR('',#7437,0.405);
#2141=VECTOR('',#7442,0.7);
#2142=VECTOR('',#7461,0.61);
#2143=VECTOR('',#7472,0.405);
#2144=VECTOR('',#7477,1.);
#2145=VECTOR('',#7490,0.3);
#2146=VECTOR('',#7499,0.3);
#2147=VECTOR('',#7508,0.225);
#2148=VECTOR('',#7515,0.225);
#2149=VECTOR('',#7522,0.225);
#2150=VECTOR('',#7529,0.225);
#2151=VECTOR('',#7536,1.01);
#2152=VECTOR('',#7541,1.);
#2153=VECTOR('',#7542,1.);
#2154=VECTOR('',#7543,1.);
#2155=VECTOR('',#7544,1.);
#2156=VECTOR('',#7547,1.);
#2157=VECTOR('',#7548,1.);
#2158=VECTOR('',#7549,1.);
#2159=VECTOR('',#7552,1.);
#2160=VECTOR('',#7553,1.);
#2161=VECTOR('',#7554,1.);
#2162=VECTOR('',#7557,1.);
#2163=VECTOR('',#7558,1.);
#2164=VECTOR('',#7573,0.75);
#2165=VECTOR('',#7580,1.3);
#2166=VECTOR('',#7591,1.);
#2167=VECTOR('',#7592,1.);
#2168=VECTOR('',#7593,1.);
#2169=VECTOR('',#7594,1.);
#2170=VECTOR('',#7597,1.);
#2171=VECTOR('',#7598,1.);
#2172=VECTOR('',#7599,1.);
#2173=VECTOR('',#7602,1.);
#2174=VECTOR('',#7603,1.);
#2175=VECTOR('',#7604,1.);
#2176=VECTOR('',#7607,1.);
#2177=VECTOR('',#7608,1.);
#2178=VECTOR('',#7609,1.);
#2179=VECTOR('',#7612,1.);
#2180=VECTOR('',#7613,1.);
#2181=VECTOR('',#7614,1.);
#2182=VECTOR('',#7617,1.);
#2183=VECTOR('',#7618,1.);
#2184=VECTOR('',#7631,0.25);
#2185=VECTOR('',#7644,0.4);
#2186=VECTOR('',#7649,0.425);
#2187=VECTOR('',#7654,0.41);
#2188=VECTOR('',#7663,0.26);
#2189=VECTOR('',#7666,0.25);
#2190=VECTOR('',#7673,0.275);
#2191=VECTOR('',#7678,0.265);
#2192=VECTOR('',#7687,0.5);
#2193=VECTOR('',#7696,0.47094010767585);
#2194=VECTOR('',#7703,0.47094010767585);
#2195=VECTOR('',#7706,1.);
#2196=VECTOR('',#7707,1.);
#2197=VECTOR('',#7710,1.);
#2198=VECTOR('',#7713,1.);
#2199=VECTOR('',#7718,0.25);
#2200=VECTOR('',#7723,1.);
#2201=VECTOR('',#7726,1.);
#2202=VECTOR('',#7737,1.);
#2203=VECTOR('',#7738,1.);
#2204=VECTOR('',#7739,1.);
#2205=VECTOR('',#7740,1.);
#2206=VECTOR('',#7741,1.);
#2207=VECTOR('',#7742,1.);
#2208=VECTOR('',#7747,1.);
#2209=VECTOR('',#7748,1.);
#2210=VECTOR('',#7749,1.);
#2211=VECTOR('',#7750,1.);
#2212=VECTOR('',#7751,1.);
#2213=VECTOR('',#7752,1.);
#2214=VECTOR('',#7757,1.);
#2215=VECTOR('',#7758,1.);
#2216=VECTOR('',#7761,1.);
#2217=VECTOR('',#7764,1.);
#2218=VECTOR('',#7767,1.);
#2219=VECTOR('',#7770,1.);
#2220=VECTOR('',#7775,1.065);
#2221=VECTOR('',#7786,1.025);
#2222=VECTOR('',#7791,1.065);
#2223=VECTOR('',#7796,1.025);
#2224=VECTOR('',#7803,0.79);
#2225=VECTOR('',#7810,0.225);
#2226=VECTOR('',#7817,0.4);
#2227=VECTOR('',#7834,0.325);
#2228=VECTOR('',#7839,0.35);
#2229=VECTOR('',#7844,0.335);
#2230=VECTOR('',#7853,0.21);
#2231=VECTOR('',#7858,0.2);
#2232=VECTOR('',#7863,0.18);
#2233=VECTOR('',#7868,1.);
#2234=VECTOR('',#7869,1.);
#2235=VECTOR('',#7870,1.);
#2236=VECTOR('',#7871,1.);
#2237=VECTOR('',#7874,1.);
#2238=VECTOR('',#7875,1.);
#2239=VECTOR('',#7876,1.);
#2240=VECTOR('',#7879,1.);
#2241=VECTOR('',#7880,1.);
#2242=VECTOR('',#7881,1.);
#2243=VECTOR('',#7884,1.);
#2244=VECTOR('',#7885,1.);
#2245=VECTOR('',#7886,1.);
#2246=VECTOR('',#7889,1.);
#2247=VECTOR('',#7890,1.);
#2248=VECTOR('',#7891,1.);
#2249=VECTOR('',#7894,1.);
#2250=VECTOR('',#7895,1.);
#2251=VECTOR('',#7906,0.3);
#2252=VECTOR('',#7921,1.);
#2253=VECTOR('',#7922,1.);
#2254=VECTOR('',#7923,1.);
#2255=VECTOR('',#7928,1.);
#2256=VECTOR('',#7929,1.);
#2257=VECTOR('',#7936,1.);
#2258=VECTOR('',#7937,1.);
#2259=VECTOR('',#7942,1.);
#2260=VECTOR('',#7949,0.75);
#2261=VECTOR('',#7962,0.165);
#2262=VECTOR('',#7971,1.);
#2263=VECTOR('',#7972,1.);
#2264=VECTOR('',#7977,1.);
#2265=VECTOR('',#7978,1.);
#2266=VECTOR('',#7983,1.);
#2267=VECTOR('',#7984,1.);
#2268=VECTOR('',#7989,1.);
#2269=VECTOR('',#7990,1.);
#2270=VECTOR('',#7993,1.);
#2271=VECTOR('',#7994,1.);
#2272=VECTOR('',#7995,1.);
#2273=VECTOR('',#7996,1.);
#2274=VECTOR('',#7999,1.);
#2275=VECTOR('',#8000,1.);
#2276=VECTOR('',#8001,1.);
#2277=VECTOR('',#8004,1.);
#2278=VECTOR('',#8005,1.);
#2279=VECTOR('',#8006,1.);
#2280=VECTOR('',#8009,1.);
#2281=VECTOR('',#8010,1.);
#2282=VECTOR('',#8033,1.);
#2283=VECTOR('',#8034,1.);
#2284=VECTOR('',#8035,1.);
#2285=VECTOR('',#8036,1.);
#2286=VECTOR('',#8039,1.);
#2287=VECTOR('',#8040,1.);
#2288=VECTOR('',#8041,1.);
#2289=VECTOR('',#8044,1.);
#2290=VECTOR('',#8045,1.);
#2291=VECTOR('',#8046,1.);
#2292=VECTOR('',#8049,1.);
#2293=VECTOR('',#8050,1.);
#2294=VECTOR('',#8055,0.4);
#2295=VECTOR('',#8064,1.);
#2296=VECTOR('',#8065,1.);
#2297=VECTOR('',#8066,1.);
#2298=VECTOR('',#8067,1.);
#2299=VECTOR('',#8070,1.);
#2300=VECTOR('',#8071,1.);
#2301=VECTOR('',#8072,1.);
#2302=VECTOR('',#8075,1.);
#2303=VECTOR('',#8076,1.);
#2304=VECTOR('',#8077,1.);
#2305=VECTOR('',#8080,1.);
#2306=VECTOR('',#8081,1.);
#2307=VECTOR('',#8084,1.);
#2308=VECTOR('',#8085,1.);
#2309=VECTOR('',#8086,1.);
#2310=VECTOR('',#8087,1.);
#2311=VECTOR('',#8090,1.);
#2312=VECTOR('',#8091,1.);
#2313=VECTOR('',#8092,1.);
#2314=VECTOR('',#8095,1.);
#2315=VECTOR('',#8096,1.);
#2316=VECTOR('',#8097,1.);
#2317=VECTOR('',#8100,1.);
#2318=VECTOR('',#8101,1.);
#2319=VECTOR('',#8112,0.225);
#2320=VECTOR('',#8119,0.6);
#2321=VECTOR('',#8130,1.);
#2322=VECTOR('',#8131,1.);
#2323=VECTOR('',#8132,1.);
#2324=VECTOR('',#8133,1.);
#2325=VECTOR('',#8136,1.);
#2326=VECTOR('',#8137,1.);
#2327=VECTOR('',#8138,1.);
#2328=VECTOR('',#8141,1.);
#2329=VECTOR('',#8142,1.);
#2330=VECTOR('',#8143,1.);
#2331=VECTOR('',#8146,1.);
#2332=VECTOR('',#8147,1.);
#2333=VECTOR('',#8156,1.);
#2334=VECTOR('',#8157,1.);
#2335=VECTOR('',#8158,1.);
#2336=VECTOR('',#8159,1.);
#2337=VECTOR('',#8162,1.);
#2338=VECTOR('',#8163,1.);
#2339=VECTOR('',#8164,1.);
#2340=VECTOR('',#8167,1.);
#2341=VECTOR('',#8168,1.);
#2342=VECTOR('',#8169,1.);
#2343=VECTOR('',#8172,1.);
#2344=VECTOR('',#8173,1.);
#2345=VECTOR('',#8174,1.);
#2346=VECTOR('',#8177,1.);
#2347=VECTOR('',#8178,1.);
#2348=VECTOR('',#8179,1.);
#2349=VECTOR('',#8182,1.);
#2350=VECTOR('',#8183,1.);
#2351=VECTOR('',#8200,0.325);
#2352=VECTOR('',#8205,0.35);
#2353=VECTOR('',#8210,0.335);
#2354=VECTOR('',#8219,0.21);
#2355=VECTOR('',#8222,0.2);
#2356=CIRCLE('',#5899,0.25);
#2357=CIRCLE('',#5900,0.25);
#2358=CIRCLE('',#5903,0.25);
#2359=CIRCLE('',#5904,0.25);
#2360=CIRCLE('',#5907,0.93);
#2361=CIRCLE('',#5908,0.93);
#2362=CIRCLE('',#5910,0.79);
#2363=CIRCLE('',#5912,0.93);
#2364=CIRCLE('',#5913,0.93);
#2365=CIRCLE('',#5915,0.79);
#2366=CIRCLE('',#5917,0.789999999999999);
#2367=CIRCLE('',#5923,0.789999999999999);
#2368=CIRCLE('',#5928,0.789999999999999);
#2369=CIRCLE('',#5932,0.789999999999999);
#2370=CIRCLE('',#5960,0.93);
#2371=CIRCLE('',#5962,0.93);
#2372=CIRCLE('',#5963,0.93);
#2373=CIRCLE('',#5966,0.789999999999999);
#2374=CIRCLE('',#5969,0.789999999999999);
#2375=CIRCLE('',#5971,0.789999999999999);
#2376=CIRCLE('',#5973,0.789999999999999);
#2377=CIRCLE('',#5976,0.93);
#2378=CIRCLE('',#5978,0.93);
#2379=CIRCLE('',#5979,0.93);
#2380=CIRCLE('',#5982,0.789999999999999);
#2381=CIRCLE('',#5985,0.789999999999999);
#2382=CIRCLE('',#5987,0.789999999999999);
#2383=CIRCLE('',#5989,0.789999999999999);
#2384=CIRCLE('',#5992,0.93);
#2385=CIRCLE('',#5994,0.93);
#2386=CIRCLE('',#5995,0.93);
#2387=CIRCLE('',#5998,0.79);
#2388=CIRCLE('',#6001,0.79);
#2389=CIRCLE('',#6003,0.79);
#2390=CIRCLE('',#6005,0.79);
#2391=CIRCLE('',#6008,0.93);
#2392=CIRCLE('',#6010,0.93);
#2393=CIRCLE('',#6011,0.93);
#2394=CIRCLE('',#6021,0.93);
#2395=CIRCLE('',#6030,0.93);
#2396=CIRCLE('',#6034,0.55);
#2397=CIRCLE('',#6035,0.55);
#2398=CIRCLE('',#6037,0.33);
#2399=CIRCLE('',#6039,0.33);
#2400=CIRCLE('',#6041,0.55);
#2401=CIRCLE('',#6042,0.55);
#2402=CIRCLE('',#6044,0.33);
#2403=CIRCLE('',#6046,0.33);
#2404=CIRCLE('',#6048,0.6);
#2405=CIRCLE('',#6049,0.6);
#2406=CIRCLE('',#6051,0.33);
#2407=CIRCLE('',#6053,0.33);
#2408=CIRCLE('',#6062,0.549999999999997);
#2409=CIRCLE('',#6063,0.549999999999997);
#2410=CIRCLE('',#6065,0.329999999999998);
#2411=CIRCLE('',#6067,0.329999999999998);
#2412=CIRCLE('',#6069,0.549999999999997);
#2413=CIRCLE('',#6070,0.549999999999997);
#2414=CIRCLE('',#6072,0.329999999999998);
#2415=CIRCLE('',#6074,0.329999999999998);
#2416=CIRCLE('',#6076,0.600000000000001);
#2417=CIRCLE('',#6077,0.600000000000001);
#2418=CIRCLE('',#6079,0.329999999999998);
#2419=CIRCLE('',#6081,0.329999999999998);
#2420=CIRCLE('',#6090,0.2942);
#2421=CIRCLE('',#6091,0.2942);
#2422=CIRCLE('',#6093,0.24);
#2423=CIRCLE('',#6096,0.475);
#2424=CIRCLE('',#6108,0.165);
#2425=CIRCLE('',#6109,0.165);
#2426=CIRCLE('',#6112,0.165);
#2427=CIRCLE('',#6113,0.165);
#2428=CIRCLE('',#6116,0.275);
#2429=CIRCLE('',#6117,0.275);
#2430=CIRCLE('',#6119,0.275);
#2431=CIRCLE('',#6120,0.275);
#2432=CIRCLE('',#6122,0.275);
#2433=CIRCLE('',#6123,0.275);
#2434=CIRCLE('',#6125,0.275);
#2435=CIRCLE('',#6126,0.275);
#2436=CIRCLE('',#6128,0.7);
#2437=CIRCLE('',#6129,0.7);
#2438=CIRCLE('',#6131,0.556776436283003);
#2439=CIRCLE('',#6134,0.93);
#2440=CIRCLE('',#6135,0.93);
#2441=CIRCLE('',#6137,1.3);
#2442=CIRCLE('',#6138,1.3);
#2443=CIRCLE('',#6140,1.24899959967968);
#2444=CIRCLE('',#6143,1.59980467557762);
#2445=CIRCLE('',#6151,0.165);
#2446=CIRCLE('',#6152,0.165);
#2447=CIRCLE('',#6155,0.165);
#2448=CIRCLE('',#6156,0.165);
#2449=CIRCLE('',#6159,0.275);
#2450=CIRCLE('',#6160,0.275);
#2451=CIRCLE('',#6162,0.275);
#2452=CIRCLE('',#6163,0.275);
#2453=CIRCLE('',#6165,0.275);
#2454=CIRCLE('',#6166,0.275);
#2455=CIRCLE('',#6168,0.275);
#2456=CIRCLE('',#6169,0.275);
#2457=CIRCLE('',#6171,0.7);
#2458=CIRCLE('',#6172,0.7);
#2459=CIRCLE('',#6174,0.556776436283003);
#2460=CIRCLE('',#6177,0.93);
#2461=CIRCLE('',#6178,0.93);
#2462=CIRCLE('',#6180,1.3);
#2463=CIRCLE('',#6181,1.3);
#2464=CIRCLE('',#6184,1.24899959967968);
#2465=CIRCLE('',#6186,1.59980467557762);
#2466=CIRCLE('',#6194,0.275);
#2467=CIRCLE('',#6195,0.275);
#2468=CIRCLE('',#6197,0.275);
#2469=CIRCLE('',#6198,0.275);
#2470=CIRCLE('',#6200,0.275);
#2471=CIRCLE('',#6201,0.275);
#2472=CIRCLE('',#6203,0.275);
#2473=CIRCLE('',#6204,0.275);
#2474=CIRCLE('',#6210,1.6);
#2475=CIRCLE('',#6214,1.6);
#2476=CIRCLE('',#6221,1.2);
#2477=CIRCLE('',#6222,0.7);
#2478=CIRCLE('',#6224,1.2);
#2479=CIRCLE('',#6226,0.405);
#2480=CIRCLE('',#6228,0.405);
#2481=CIRCLE('',#6230,0.7);
#2482=CIRCLE('',#6234,0.1);
#2483=CIRCLE('',#6235,0.4);
#2484=CIRCLE('',#6238,0.61);
#2485=CIRCLE('',#6239,0.61);
#2486=CIRCLE('',#6241,0.405);
#2487=CIRCLE('',#6243,0.405);
#2488=CIRCLE('',#6245,1.);
#2489=CIRCLE('',#6246,1.);
#2490=CIRCLE('',#6251,0.3);
#2491=CIRCLE('',#6252,0.3);
#2492=CIRCLE('',#6255,0.3);
#2493=CIRCLE('',#6256,0.3);
#2494=CIRCLE('',#6259,0.225);
#2495=CIRCLE('',#6260,0.225);
#2496=CIRCLE('',#6262,0.225);
#2497=CIRCLE('',#6263,0.225);
#2498=CIRCLE('',#6265,0.225);
#2499=CIRCLE('',#6266,0.225);
#2500=CIRCLE('',#6268,0.225);
#2501=CIRCLE('',#6269,0.225);
#2502=CIRCLE('',#6271,1.01);
#2503=CIRCLE('',#6272,1.01);
#2504=CIRCLE('',#6281,1.11803398874989);
#2505=CIRCLE('',#6282,0.75);
#2506=CIRCLE('',#6284,0.75);
#2507=CIRCLE('',#6286,1.3);
#2508=CIRCLE('',#6287,1.3);
#2509=CIRCLE('',#6300,0.25);
#2510=CIRCLE('',#6301,0.24505);
#2511=CIRCLE('',#6303,0.25);
#2512=CIRCLE('',#6306,0.375);
#2513=CIRCLE('',#6308,0.425);
#2514=CIRCLE('',#6310,0.425);
#2515=CIRCLE('',#6312,0.395);
#2516=CIRCLE('',#6314,0.27);
#2517=CIRCLE('',#6316,0.24505);
#2518=CIRCLE('',#6320,0.285);
#2519=CIRCLE('',#6321,0.265);
#2520=CIRCLE('',#6323,0.265);
#2521=CIRCLE('',#6325,0.5);
#2522=CIRCLE('',#6327,0.5);
#2523=CIRCLE('',#6331,0.38);
#2524=CIRCLE('',#6333,0.38);
#2525=CIRCLE('',#6338,0.2117);
#2526=CIRCLE('',#6339,0.2117);
#2527=CIRCLE('',#6347,1.065);
#2528=CIRCLE('',#6349,1.065);
#2529=CIRCLE('',#6357,1.065);
#2530=CIRCLE('',#6359,0.985);
#2531=CIRCLE('',#6360,0.79);
#2532=CIRCLE('',#6363,1.065);
#2533=CIRCLE('',#6365,0.985);
#2534=CIRCLE('',#6367,0.79);
#2535=CIRCLE('',#6371,0.225);
#2536=CIRCLE('',#6372,0.225);
#2537=CIRCLE('',#6374,0.4);
#2538=CIRCLE('',#6375,0.4);
#2539=CIRCLE('',#6380,0.3);
#2540=CIRCLE('',#6382,0.35);
#2541=CIRCLE('',#6384,0.35);
#2542=CIRCLE('',#6386,0.32);
#2543=CIRCLE('',#6388,0.22);
#2544=CIRCLE('',#6390,0.1954);
#2545=CIRCLE('',#6392,0.1954);
#2546=CIRCLE('',#6394,0.16);
#2547=CIRCLE('',#6406,0.3);
#2548=CIRCLE('',#6407,0.3);
#2549=CIRCLE('',#6413,1.48592563743951);
#2550=CIRCLE('',#6415,1.48592563743951);
#2551=CIRCLE('',#6416,1.48592563743951);
#2552=CIRCLE('',#6418,1.48592563743951);
#2553=CIRCLE('',#6420,1.48592563743951);
#2554=CIRCLE('',#6423,0.75);
#2555=CIRCLE('',#6424,0.75);
#2556=CIRCLE('',#6426,1.5);
#2557=CIRCLE('',#6429,0.165);
#2558=CIRCLE('',#6430,0.165);
#2559=CIRCLE('',#6433,0.4);
#2560=CIRCLE('',#6435,0.4);
#2561=CIRCLE('',#6437,0.4);
#2562=CIRCLE('',#6439,0.4);
#2563=CIRCLE('',#6446,0.4);
#2564=CIRCLE('',#6448,0.4);
#2565=CIRCLE('',#6449,0.4);
#2566=CIRCLE('',#6451,0.4);
#2567=CIRCLE('',#6453,0.4);
#2568=CIRCLE('',#6460,0.4);
#2569=CIRCLE('',#6475,0.225);
#2570=CIRCLE('',#6476,0.225);
#2571=CIRCLE('',#6478,0.6);
#2572=CIRCLE('',#6479,0.6);
#2573=CIRCLE('',#6499,0.1954);
#2574=CIRCLE('',#6501,0.3);
#2575=CIRCLE('',#6503,0.35);
#2576=CIRCLE('',#6505,0.35);
#2577=CIRCLE('',#6507,0.32);
#2578=CIRCLE('',#6509,0.22);
#2579=CIRCLE('',#6511,0.1954);
#2580=VERTEX_POINT('',#8339);
#2581=VERTEX_POINT('',#8341);
#2582=VERTEX_POINT('',#8346);
#2583=VERTEX_POINT('',#8348);
#2584=VERTEX_POINT('',#8353);
#2585=VERTEX_POINT('',#8355);
#2586=VERTEX_POINT('',#8359);
#2587=VERTEX_POINT('',#8362);
#2588=VERTEX_POINT('',#8364);
#2589=VERTEX_POINT('',#8368);
#2590=VERTEX_POINT('',#8371);
#2591=VERTEX_POINT('',#8372);
#2592=VERTEX_POINT('',#8376);
#2593=VERTEX_POINT('',#8380);
#2594=VERTEX_POINT('',#8381);
#2595=VERTEX_POINT('',#8383);
#2596=VERTEX_POINT('',#8387);
#2597=VERTEX_POINT('',#8389);
#2598=VERTEX_POINT('',#8393);
#2599=VERTEX_POINT('',#8395);
#2600=VERTEX_POINT('',#8401);
#2601=VERTEX_POINT('',#8403);
#2602=VERTEX_POINT('',#8405);
#2603=VERTEX_POINT('',#8407);
#2604=VERTEX_POINT('',#8416);
#2605=VERTEX_POINT('',#8425);
#2606=VERTEX_POINT('',#8427);
#2607=VERTEX_POINT('',#8429);
#2608=VERTEX_POINT('',#8431);
#2609=VERTEX_POINT('',#8434);
#2610=VERTEX_POINT('',#8436);
#2611=VERTEX_POINT('',#8438);
#2612=VERTEX_POINT('',#8453);
#2613=VERTEX_POINT('',#8456);
#2614=VERTEX_POINT('',#8458);
#2615=VERTEX_POINT('',#8460);
#2616=VERTEX_POINT('',#8462);
#2617=VERTEX_POINT('',#8471);
#2618=VERTEX_POINT('',#8480);
#2619=VERTEX_POINT('',#8482);
#2620=VERTEX_POINT('',#8484);
#2621=VERTEX_POINT('',#8486);
#2622=VERTEX_POINT('',#8489);
#2623=VERTEX_POINT('',#8491);
#2624=VERTEX_POINT('',#8493);
#2625=VERTEX_POINT('',#8508);
#2626=VERTEX_POINT('',#8511);
#2627=VERTEX_POINT('',#8513);
#2628=VERTEX_POINT('',#8515);
#2629=VERTEX_POINT('',#8517);
#2630=VERTEX_POINT('',#8526);
#2631=VERTEX_POINT('',#8535);
#2632=VERTEX_POINT('',#8537);
#2633=VERTEX_POINT('',#8539);
#2634=VERTEX_POINT('',#8541);
#2635=VERTEX_POINT('',#8544);
#2636=VERTEX_POINT('',#8546);
#2637=VERTEX_POINT('',#8548);
#2638=VERTEX_POINT('',#8563);
#2639=VERTEX_POINT('',#8567);
#2640=VERTEX_POINT('',#8569);
#2641=VERTEX_POINT('',#8578);
#2642=VERTEX_POINT('',#8588);
#2643=VERTEX_POINT('',#8590);
#2644=VERTEX_POINT('',#8607);
#2645=VERTEX_POINT('',#8609);
#2646=VERTEX_POINT('',#8612);
#2647=VERTEX_POINT('',#8614);
#2648=VERTEX_POINT('',#8617);
#2649=VERTEX_POINT('',#8619);
#2650=VERTEX_POINT('',#8625);
#2651=VERTEX_POINT('',#8643);
#2652=VERTEX_POINT('',#8661);
#2653=VERTEX_POINT('',#8679);
#2654=VERTEX_POINT('',#8685);
#2655=VERTEX_POINT('',#8686);
#2656=VERTEX_POINT('',#8688);
#2657=VERTEX_POINT('',#8690);
#2658=VERTEX_POINT('',#8694);
#2659=VERTEX_POINT('',#8696);
#2660=VERTEX_POINT('',#8700);
#2661=VERTEX_POINT('',#8702);
#2662=VERTEX_POINT('',#8712);
#2663=VERTEX_POINT('',#8713);
#2664=VERTEX_POINT('',#8715);
#2665=VERTEX_POINT('',#8717);
#2666=VERTEX_POINT('',#8719);
#2667=VERTEX_POINT('',#8721);
#2668=VERTEX_POINT('',#8724);
#2669=VERTEX_POINT('',#8727);
#2670=VERTEX_POINT('',#8728);
#2671=VERTEX_POINT('',#8733);
#2672=VERTEX_POINT('',#8737);
#2673=VERTEX_POINT('',#8741);
#2674=VERTEX_POINT('',#8745);
#2675=VERTEX_POINT('',#8752);
#2676=VERTEX_POINT('',#8758);
#2677=VERTEX_POINT('',#8760);
#2678=VERTEX_POINT('',#8764);
#2679=VERTEX_POINT('',#8767);
#2680=VERTEX_POINT('',#8771);
#2681=VERTEX_POINT('',#8773);
#2682=VERTEX_POINT('',#8777);
#2683=VERTEX_POINT('',#8780);
#2684=VERTEX_POINT('',#8784);
#2685=VERTEX_POINT('',#8786);
#2686=VERTEX_POINT('',#8790);
#2687=VERTEX_POINT('',#8793);
#2688=VERTEX_POINT('',#8797);
#2689=VERTEX_POINT('',#8798);
#2690=VERTEX_POINT('',#8800);
#2691=VERTEX_POINT('',#8802);
#2692=VERTEX_POINT('',#8806);
#2693=VERTEX_POINT('',#8808);
#2694=VERTEX_POINT('',#8812);
#2695=VERTEX_POINT('',#8814);
#2696=VERTEX_POINT('',#8824);
#2697=VERTEX_POINT('',#8826);
#2698=VERTEX_POINT('',#8830);
#2699=VERTEX_POINT('',#8833);
#2700=VERTEX_POINT('',#8837);
#2701=VERTEX_POINT('',#8839);
#2702=VERTEX_POINT('',#8843);
#2703=VERTEX_POINT('',#8846);
#2704=VERTEX_POINT('',#8850);
#2705=VERTEX_POINT('',#8852);
#2706=VERTEX_POINT('',#8856);
#2707=VERTEX_POINT('',#8859);
#2708=VERTEX_POINT('',#8863);
#2709=VERTEX_POINT('',#8864);
#2710=VERTEX_POINT('',#8866);
#2711=VERTEX_POINT('',#8868);
#2712=VERTEX_POINT('',#8872);
#2713=VERTEX_POINT('',#8874);
#2714=VERTEX_POINT('',#8878);
#2715=VERTEX_POINT('',#8880);
#2716=VERTEX_POINT('',#8890);
#2717=VERTEX_POINT('',#8892);
#2718=VERTEX_POINT('',#8896);
#2719=VERTEX_POINT('',#8901);
#2720=VERTEX_POINT('',#8903);
#2721=VERTEX_POINT('',#8905);
#2722=VERTEX_POINT('',#8909);
#2723=VERTEX_POINT('',#8913);
#2724=VERTEX_POINT('',#8917);
#2725=VERTEX_POINT('',#8921);
#2726=VERTEX_POINT('',#8929);
#2727=VERTEX_POINT('',#8931);
#2728=VERTEX_POINT('',#8935);
#2729=VERTEX_POINT('',#8939);
#2730=VERTEX_POINT('',#8943);
#2731=VERTEX_POINT('',#8947);
#2732=VERTEX_POINT('',#8957);
#2733=VERTEX_POINT('',#8959);
#2734=VERTEX_POINT('',#8964);
#2735=VERTEX_POINT('',#8966);
#2736=VERTEX_POINT('',#8971);
#2737=VERTEX_POINT('',#8973);
#2738=VERTEX_POINT('',#8977);
#2739=VERTEX_POINT('',#8979);
#2740=VERTEX_POINT('',#8983);
#2741=VERTEX_POINT('',#8985);
#2742=VERTEX_POINT('',#8989);
#2743=VERTEX_POINT('',#8991);
#2744=VERTEX_POINT('',#8995);
#2745=VERTEX_POINT('',#8996);
#2746=VERTEX_POINT('',#8998);
#2747=VERTEX_POINT('',#9000);
#2748=VERTEX_POINT('',#9004);
#2749=VERTEX_POINT('',#9006);
#2750=VERTEX_POINT('',#9010);
#2751=VERTEX_POINT('',#9012);
#2752=VERTEX_POINT('',#9014);
#2753=VERTEX_POINT('',#9016);
#2754=VERTEX_POINT('',#9020);
#2755=VERTEX_POINT('',#9022);
#2756=VERTEX_POINT('',#9026);
#2757=VERTEX_POINT('',#9028);
#2758=VERTEX_POINT('',#9032);
#2759=VERTEX_POINT('',#9038);
#2760=VERTEX_POINT('',#9040);
#2761=VERTEX_POINT('',#9044);
#2762=VERTEX_POINT('',#9048);
#2763=VERTEX_POINT('',#9056);
#2764=VERTEX_POINT('',#9058);
#2765=VERTEX_POINT('',#9063);
#2766=VERTEX_POINT('',#9065);
#2767=VERTEX_POINT('',#9070);
#2768=VERTEX_POINT('',#9072);
#2769=VERTEX_POINT('',#9076);
#2770=VERTEX_POINT('',#9078);
#2771=VERTEX_POINT('',#9082);
#2772=VERTEX_POINT('',#9084);
#2773=VERTEX_POINT('',#9088);
#2774=VERTEX_POINT('',#9090);
#2775=VERTEX_POINT('',#9094);
#2776=VERTEX_POINT('',#9095);
#2777=VERTEX_POINT('',#9097);
#2778=VERTEX_POINT('',#9099);
#2779=VERTEX_POINT('',#9103);
#2780=VERTEX_POINT('',#9105);
#2781=VERTEX_POINT('',#9109);
#2782=VERTEX_POINT('',#9111);
#2783=VERTEX_POINT('',#9113);
#2784=VERTEX_POINT('',#9115);
#2785=VERTEX_POINT('',#9119);
#2786=VERTEX_POINT('',#9121);
#2787=VERTEX_POINT('',#9125);
#2788=VERTEX_POINT('',#9127);
#2789=VERTEX_POINT('',#9132);
#2790=VERTEX_POINT('',#9137);
#2791=VERTEX_POINT('',#9138);
#2792=VERTEX_POINT('',#9143);
#2793=VERTEX_POINT('',#9147);
#2794=VERTEX_POINT('',#9155);
#2795=VERTEX_POINT('',#9157);
#2796=VERTEX_POINT('',#9161);
#2797=VERTEX_POINT('',#9163);
#2798=VERTEX_POINT('',#9167);
#2799=VERTEX_POINT('',#9169);
#2800=VERTEX_POINT('',#9173);
#2801=VERTEX_POINT('',#9175);
#2802=VERTEX_POINT('',#9179);
#2803=VERTEX_POINT('',#9180);
#2804=VERTEX_POINT('',#9182);
#2805=VERTEX_POINT('',#9184);
#2806=VERTEX_POINT('',#9188);
#2807=VERTEX_POINT('',#9189);
#2808=VERTEX_POINT('',#9191);
#2809=VERTEX_POINT('',#9193);
#2810=VERTEX_POINT('',#9197);
#2811=VERTEX_POINT('',#9199);
#2812=VERTEX_POINT('',#9203);
#2813=VERTEX_POINT('',#9205);
#2814=VERTEX_POINT('',#9210);
#2815=VERTEX_POINT('',#9212);
#2816=VERTEX_POINT('',#9214);
#2817=VERTEX_POINT('',#9216);
#2818=VERTEX_POINT('',#9220);
#2819=VERTEX_POINT('',#9224);
#2820=VERTEX_POINT('',#9230);
#2821=VERTEX_POINT('',#9234);
#2822=VERTEX_POINT('',#9242);
#2823=VERTEX_POINT('',#9244);
#2824=VERTEX_POINT('',#9247);
#2825=VERTEX_POINT('',#9251);
#2826=VERTEX_POINT('',#9254);
#2827=VERTEX_POINT('',#9258);
#2828=VERTEX_POINT('',#9264);
#2829=VERTEX_POINT('',#9269);
#2830=VERTEX_POINT('',#9271);
#2831=VERTEX_POINT('',#9275);
#2832=VERTEX_POINT('',#9278);
#2833=VERTEX_POINT('',#9282);
#2834=VERTEX_POINT('',#9284);
#2835=VERTEX_POINT('',#9291);
#2836=VERTEX_POINT('',#9293);
#2837=VERTEX_POINT('',#9298);
#2838=VERTEX_POINT('',#9300);
#2839=VERTEX_POINT('',#9305);
#2840=VERTEX_POINT('',#9307);
#2841=VERTEX_POINT('',#9311);
#2842=VERTEX_POINT('',#9313);
#2843=VERTEX_POINT('',#9317);
#2844=VERTEX_POINT('',#9319);
#2845=VERTEX_POINT('',#9323);
#2846=VERTEX_POINT('',#9325);
#2847=VERTEX_POINT('',#9329);
#2848=VERTEX_POINT('',#9331);
#2849=VERTEX_POINT('',#9335);
#2850=VERTEX_POINT('',#9336);
#2851=VERTEX_POINT('',#9338);
#2852=VERTEX_POINT('',#9340);
#2853=VERTEX_POINT('',#9344);
#2854=VERTEX_POINT('',#9346);
#2855=VERTEX_POINT('',#9350);
#2856=VERTEX_POINT('',#9352);
#2857=VERTEX_POINT('',#9362);
#2858=VERTEX_POINT('',#9364);
#2859=VERTEX_POINT('',#9367);
#2860=VERTEX_POINT('',#9371);
#2861=VERTEX_POINT('',#9373);
#2862=VERTEX_POINT('',#9380);
#2863=VERTEX_POINT('',#9381);
#2864=VERTEX_POINT('',#9383);
#2865=VERTEX_POINT('',#9385);
#2866=VERTEX_POINT('',#9389);
#2867=VERTEX_POINT('',#9391);
#2868=VERTEX_POINT('',#9395);
#2869=VERTEX_POINT('',#9397);
#2870=VERTEX_POINT('',#9401);
#2871=VERTEX_POINT('',#9403);
#2872=VERTEX_POINT('',#9407);
#2873=VERTEX_POINT('',#9409);
#2874=VERTEX_POINT('',#9418);
#2875=VERTEX_POINT('',#9420);
#2876=VERTEX_POINT('',#9423);
#2877=VERTEX_POINT('',#9428);
#2878=VERTEX_POINT('',#9431);
#2879=VERTEX_POINT('',#9435);
#2880=VERTEX_POINT('',#9439);
#2881=VERTEX_POINT('',#9443);
#2882=VERTEX_POINT('',#9446);
#2883=VERTEX_POINT('',#9453);
#2884=VERTEX_POINT('',#9455);
#2885=VERTEX_POINT('',#9459);
#2886=VERTEX_POINT('',#9463);
#2887=VERTEX_POINT('',#9466);
#2888=VERTEX_POINT('',#9472);
#2889=VERTEX_POINT('',#9473);
#2890=VERTEX_POINT('',#9477);
#2891=VERTEX_POINT('',#9481);
#2892=VERTEX_POINT('',#9484);
#2893=VERTEX_POINT('',#9488);
#2894=VERTEX_POINT('',#9492);
#2895=VERTEX_POINT('',#9500);
#2896=VERTEX_POINT('',#9502);
#2897=VERTEX_POINT('',#9504);
#2898=VERTEX_POINT('',#9508);
#2899=VERTEX_POINT('',#9512);
#2900=VERTEX_POINT('',#9516);
#2901=VERTEX_POINT('',#9520);
#2902=VERTEX_POINT('',#9535);
#2903=VERTEX_POINT('',#9537);
#2904=VERTEX_POINT('',#9549);
#2905=VERTEX_POINT('',#9550);
#2906=VERTEX_POINT('',#9552);
#2907=VERTEX_POINT('',#9554);
#2908=VERTEX_POINT('',#9556);
#2909=VERTEX_POINT('',#9558);
#2910=VERTEX_POINT('',#9561);
#2911=VERTEX_POINT('',#9564);
#2912=VERTEX_POINT('',#9565);
#2913=VERTEX_POINT('',#9567);
#2914=VERTEX_POINT('',#9569);
#2915=VERTEX_POINT('',#9571);
#2916=VERTEX_POINT('',#9573);
#2917=VERTEX_POINT('',#9576);
#2918=VERTEX_POINT('',#9591);
#2919=VERTEX_POINT('',#9595);
#2920=VERTEX_POINT('',#9597);
#2921=VERTEX_POINT('',#9602);
#2922=VERTEX_POINT('',#9606);
#2923=VERTEX_POINT('',#9610);
#2924=VERTEX_POINT('',#9616);
#2925=VERTEX_POINT('',#9618);
#2926=VERTEX_POINT('',#9622);
#2927=VERTEX_POINT('',#9624);
#2928=VERTEX_POINT('',#9631);
#2929=VERTEX_POINT('',#9634);
#2930=VERTEX_POINT('',#9638);
#2931=VERTEX_POINT('',#9642);
#2932=VERTEX_POINT('',#9646);
#2933=VERTEX_POINT('',#9649);
#2934=VERTEX_POINT('',#9653);
#2935=VERTEX_POINT('',#9657);
#2936=VERTEX_POINT('',#9662);
#2937=VERTEX_POINT('',#9663);
#2938=VERTEX_POINT('',#9665);
#2939=VERTEX_POINT('',#9667);
#2940=VERTEX_POINT('',#9671);
#2941=VERTEX_POINT('',#9673);
#2942=VERTEX_POINT('',#9677);
#2943=VERTEX_POINT('',#9679);
#2944=VERTEX_POINT('',#9683);
#2945=VERTEX_POINT('',#9685);
#2946=VERTEX_POINT('',#9689);
#2947=VERTEX_POINT('',#9691);
#2948=VERTEX_POINT('',#9701);
#2949=VERTEX_POINT('',#9703);
#2950=VERTEX_POINT('',#9711);
#2951=VERTEX_POINT('',#9712);
#2952=VERTEX_POINT('',#9714);
#2953=VERTEX_POINT('',#9716);
#2954=VERTEX_POINT('',#9720);
#2955=VERTEX_POINT('',#9722);
#2956=VERTEX_POINT('',#9724);
#2957=VERTEX_POINT('',#9728);
#2958=VERTEX_POINT('',#9730);
#2959=VERTEX_POINT('',#9738);
#2960=VERTEX_POINT('',#9740);
#2961=VERTEX_POINT('',#9744);
#2962=VERTEX_POINT('',#9748);
#2963=VERTEX_POINT('',#9750);
#2964=VERTEX_POINT('',#9755);
#2965=VERTEX_POINT('',#9756);
#2966=VERTEX_POINT('',#9758);
#2967=VERTEX_POINT('',#9762);
#2968=VERTEX_POINT('',#9763);
#2969=VERTEX_POINT('',#9765);
#2970=VERTEX_POINT('',#9769);
#2971=VERTEX_POINT('',#9770);
#2972=VERTEX_POINT('',#9772);
#2973=VERTEX_POINT('',#9776);
#2974=VERTEX_POINT('',#9777);
#2975=VERTEX_POINT('',#9779);
#2976=VERTEX_POINT('',#9784);
#2977=VERTEX_POINT('',#9786);
#2978=VERTEX_POINT('',#9791);
#2979=VERTEX_POINT('',#9796);
#2980=VERTEX_POINT('',#9806);
#2981=VERTEX_POINT('',#9814);
#2982=VERTEX_POINT('',#9815);
#2983=VERTEX_POINT('',#9817);
#2984=VERTEX_POINT('',#9819);
#2985=VERTEX_POINT('',#9823);
#2986=VERTEX_POINT('',#9825);
#2987=VERTEX_POINT('',#9829);
#2988=VERTEX_POINT('',#9831);
#2989=VERTEX_POINT('',#9839);
#2990=VERTEX_POINT('',#9845);
#2991=VERTEX_POINT('',#9846);
#2992=VERTEX_POINT('',#9848);
#2993=VERTEX_POINT('',#9850);
#2994=VERTEX_POINT('',#9854);
#2995=VERTEX_POINT('',#9856);
#2996=VERTEX_POINT('',#9860);
#2997=VERTEX_POINT('',#9862);
#2998=VERTEX_POINT('',#9869);
#2999=VERTEX_POINT('',#9870);
#3000=VERTEX_POINT('',#9872);
#3001=VERTEX_POINT('',#9874);
#3002=VERTEX_POINT('',#9878);
#3003=VERTEX_POINT('',#9880);
#3004=VERTEX_POINT('',#9884);
#3005=VERTEX_POINT('',#9886);
#3006=VERTEX_POINT('',#9896);
#3007=VERTEX_POINT('',#9898);
#3008=VERTEX_POINT('',#9902);
#3009=VERTEX_POINT('',#9904);
#3010=VERTEX_POINT('',#9911);
#3011=VERTEX_POINT('',#9912);
#3012=VERTEX_POINT('',#9914);
#3013=VERTEX_POINT('',#9916);
#3014=VERTEX_POINT('',#9920);
#3015=VERTEX_POINT('',#9922);
#3016=VERTEX_POINT('',#9926);
#3017=VERTEX_POINT('',#9928);
#3018=VERTEX_POINT('',#9938);
#3019=VERTEX_POINT('',#9939);
#3020=VERTEX_POINT('',#9941);
#3021=VERTEX_POINT('',#9943);
#3022=VERTEX_POINT('',#9947);
#3023=VERTEX_POINT('',#9949);
#3024=VERTEX_POINT('',#9953);
#3025=VERTEX_POINT('',#9955);
#3026=VERTEX_POINT('',#9959);
#3027=VERTEX_POINT('',#9961);
#3028=VERTEX_POINT('',#9965);
#3029=VERTEX_POINT('',#9967);
#3030=VERTEX_POINT('',#9976);
#3031=VERTEX_POINT('',#9979);
#3032=VERTEX_POINT('',#9982);
#3033=VERTEX_POINT('',#9986);
#3034=VERTEX_POINT('',#9990);
#3035=VERTEX_POINT('',#9994);
#3036=VERTEX_POINT('',#9997);
#3037=EDGE_CURVE('',#2580,#2580,#2356,.T.);
#3038=EDGE_CURVE('',#2580,#2581,#1520,.T.);
#3039=EDGE_CURVE('',#2581,#2581,#2357,.T.);
#3040=EDGE_CURVE('',#2582,#2582,#2358,.T.);
#3041=EDGE_CURVE('',#2582,#2583,#1521,.T.);
#3042=EDGE_CURVE('',#2583,#2583,#2359,.T.);
#3043=EDGE_CURVE('',#2584,#2584,#2360,.T.);
#3044=EDGE_CURVE('',#2584,#2585,#1522,.T.);
#3045=EDGE_CURVE('',#2585,#2585,#2361,.T.);
#3046=EDGE_CURVE('',#2586,#2586,#2362,.T.);
#3047=EDGE_CURVE('',#2587,#2587,#2363,.T.);
#3048=EDGE_CURVE('',#2587,#2588,#1523,.T.);
#3049=EDGE_CURVE('',#2588,#2588,#2364,.T.);
#3050=EDGE_CURVE('',#2589,#2589,#2365,.T.);
#3051=EDGE_CURVE('',#2590,#2591,#1524,.T.);
#3052=EDGE_CURVE('',#2591,#2590,#2366,.T.);
#3053=EDGE_CURVE('',#2591,#2592,#394,.T.);
#3054=EDGE_CURVE('',#2592,#2590,#395,.T.);
#3055=EDGE_CURVE('',#2593,#2594,#396,.T.);
#3056=EDGE_CURVE('',#2593,#2595,#2367,.T.);
#3057=EDGE_CURVE('',#2594,#2595,#397,.T.);
#3058=EDGE_CURVE('',#2592,#2596,#398,.T.);
#3059=EDGE_CURVE('',#2597,#2592,#399,.T.);
#3060=EDGE_CURVE('',#2596,#2597,#2368,.T.);
#3061=EDGE_CURVE('',#2594,#2598,#400,.T.);
#3062=EDGE_CURVE('',#2599,#2594,#401,.T.);
#3063=EDGE_CURVE('',#2598,#2599,#2369,.T.);
#3064=EDGE_CURVE('',#2595,#2593,#1525,.T.);
#3065=EDGE_CURVE('',#2589,#2600,#1526,.T.);
#3066=EDGE_CURVE('',#2600,#2601,#402,.T.);
#3067=EDGE_CURVE('',#2601,#2602,#1527,.T.);
#3068=EDGE_CURVE('',#2602,#2603,#382,.T.);
#3069=EDGE_CURVE('',#2603,#2604,#383,.T.);
#3070=EDGE_CURVE('',#2604,#2605,#1528,.T.);
#3071=EDGE_CURVE('',#2605,#2606,#403,.T.);
#3072=EDGE_CURVE('',#2606,#2607,#404,.T.);
#3073=EDGE_CURVE('',#2607,#2608,#1529,.T.);
#3074=EDGE_CURVE('',#2608,#2606,#405,.T.);
#3075=EDGE_CURVE('',#2606,#2609,#406,.T.);
#3076=EDGE_CURVE('',#2609,#2610,#1530,.T.);
#3077=EDGE_CURVE('',#2610,#2611,#384,.T.);
#3078=EDGE_CURVE('',#2611,#2612,#1531,.T.);
#3079=EDGE_CURVE('',#2612,#2600,#407,.T.);
#3080=EDGE_CURVE('',#2600,#2613,#1532,.T.);
#3081=EDGE_CURVE('',#2613,#2614,#408,.T.);
#3082=EDGE_CURVE('',#2614,#2615,#1533,.T.);
#3083=EDGE_CURVE('',#2615,#2616,#385,.T.);
#3084=EDGE_CURVE('',#2616,#2617,#386,.T.);
#3085=EDGE_CURVE('',#2617,#2618,#1534,.T.);
#3086=EDGE_CURVE('',#2618,#2619,#409,.T.);
#3087=EDGE_CURVE('',#2619,#2620,#410,.T.);
#3088=EDGE_CURVE('',#2620,#2621,#1535,.T.);
#3089=EDGE_CURVE('',#2621,#2619,#411,.T.);
#3090=EDGE_CURVE('',#2619,#2622,#412,.T.);
#3091=EDGE_CURVE('',#2622,#2623,#1536,.T.);
#3092=EDGE_CURVE('',#2623,#2624,#387,.T.);
#3093=EDGE_CURVE('',#2624,#2625,#1537,.T.);
#3094=EDGE_CURVE('',#2625,#2613,#413,.T.);
#3095=EDGE_CURVE('',#2613,#2626,#1538,.T.);
#3096=EDGE_CURVE('',#2626,#2627,#414,.T.);
#3097=EDGE_CURVE('',#2627,#2628,#1539,.T.);
#3098=EDGE_CURVE('',#2628,#2629,#388,.T.);
#3099=EDGE_CURVE('',#2629,#2630,#389,.T.);
#3100=EDGE_CURVE('',#2630,#2631,#1540,.T.);
#3101=EDGE_CURVE('',#2631,#2632,#415,.T.);
#3102=EDGE_CURVE('',#2632,#2633,#416,.T.);
#3103=EDGE_CURVE('',#2633,#2634,#1541,.T.);
#3104=EDGE_CURVE('',#2634,#2632,#417,.T.);
#3105=EDGE_CURVE('',#2632,#2635,#418,.T.);
#3106=EDGE_CURVE('',#2635,#2636,#1542,.T.);
#3107=EDGE_CURVE('',#2636,#2637,#390,.T.);
#3108=EDGE_CURVE('',#2637,#2638,#1543,.T.);
#3109=EDGE_CURVE('',#2638,#2626,#419,.T.);
#3110=EDGE_CURVE('',#2626,#2594,#1544,.T.);
#3111=EDGE_CURVE('',#2598,#2639,#1545,.T.);
#3112=EDGE_CURVE('',#2639,#2640,#391,.T.);
#3113=EDGE_CURVE('',#2640,#2641,#392,.T.);
#3114=EDGE_CURVE('',#2641,#2597,#1546,.T.);
#3115=EDGE_CURVE('',#2596,#2642,#1547,.T.);
#3116=EDGE_CURVE('',#2642,#2643,#393,.T.);
#3117=EDGE_CURVE('',#2643,#2599,#1548,.T.);
#3118=EDGE_CURVE('',#2594,#2586,#1549,.T.);
#3119=EDGE_CURVE('',#2626,#2644,#420,.T.);
#3120=EDGE_CURVE('',#2644,#2645,#1550,.T.);
#3121=EDGE_CURVE('',#2645,#2626,#421,.T.);
#3122=EDGE_CURVE('',#2613,#2646,#422,.T.);
#3123=EDGE_CURVE('',#2646,#2647,#1551,.T.);
#3124=EDGE_CURVE('',#2647,#2613,#423,.T.);
#3125=EDGE_CURVE('',#2600,#2648,#424,.T.);
#3126=EDGE_CURVE('',#2648,#2649,#1552,.T.);
#3127=EDGE_CURVE('',#2649,#2600,#425,.T.);
#3128=EDGE_CURVE('',#2639,#2643,#2370,.T.);
#3129=EDGE_CURVE('',#2650,#2650,#2371,.T.);
#3130=EDGE_CURVE('',#2650,#2640,#1553,.T.);
#3131=EDGE_CURVE('',#2642,#2641,#2372,.T.);
#3132=EDGE_CURVE('',#2634,#2633,#2373,.T.);
#3133=EDGE_CURVE('',#2645,#2644,#2374,.T.);
#3134=EDGE_CURVE('',#2635,#2631,#2375,.T.);
#3135=EDGE_CURVE('',#2627,#2638,#2376,.T.);
#3136=EDGE_CURVE('',#2628,#2637,#2377,.T.);
#3137=EDGE_CURVE('',#2651,#2651,#2378,.T.);
#3138=EDGE_CURVE('',#2651,#2629,#1554,.T.);
#3139=EDGE_CURVE('',#2636,#2630,#2379,.T.);
#3140=EDGE_CURVE('',#2621,#2620,#2380,.T.);
#3141=EDGE_CURVE('',#2647,#2646,#2381,.T.);
#3142=EDGE_CURVE('',#2622,#2618,#2382,.T.);
#3143=EDGE_CURVE('',#2614,#2625,#2383,.T.);
#3144=EDGE_CURVE('',#2615,#2624,#2384,.T.);
#3145=EDGE_CURVE('',#2652,#2652,#2385,.T.);
#3146=EDGE_CURVE('',#2652,#2616,#1555,.T.);
#3147=EDGE_CURVE('',#2623,#2617,#2386,.T.);
#3148=EDGE_CURVE('',#2608,#2607,#2387,.T.);
#3149=EDGE_CURVE('',#2649,#2648,#2388,.T.);
#3150=EDGE_CURVE('',#2609,#2605,#2389,.T.);
#3151=EDGE_CURVE('',#2601,#2612,#2390,.T.);
#3152=EDGE_CURVE('',#2602,#2611,#2391,.T.);
#3153=EDGE_CURVE('',#2653,#2653,#2392,.T.);
#3154=EDGE_CURVE('',#2653,#2603,#1556,.T.);
#3155=EDGE_CURVE('',#2610,#2604,#2393,.T.);
#3156=EDGE_CURVE('',#2654,#2655,#1557,.T.);
#3157=EDGE_CURVE('',#2655,#2656,#1558,.T.);
#3158=EDGE_CURVE('',#2657,#2656,#1559,.T.);
#3159=EDGE_CURVE('',#2654,#2657,#1560,.T.);
#3160=EDGE_CURVE('',#2658,#2654,#1561,.T.);
#3161=EDGE_CURVE('',#2659,#2657,#1562,.T.);
#3162=EDGE_CURVE('',#2658,#2659,#1563,.T.);
#3163=EDGE_CURVE('',#2660,#2658,#1564,.T.);
#3164=EDGE_CURVE('',#2661,#2659,#1565,.T.);
#3165=EDGE_CURVE('',#2660,#2661,#1566,.T.);
#3166=EDGE_CURVE('',#2655,#2660,#1567,.T.);
#3167=EDGE_CURVE('',#2656,#2661,#1568,.T.);
#3168=EDGE_CURVE('',#2662,#2663,#1569,.T.);
#3169=EDGE_CURVE('',#2663,#2664,#1570,.T.);
#3170=EDGE_CURVE('',#2664,#2665,#1571,.T.);
#3171=EDGE_CURVE('',#2665,#2666,#1572,.T.);
#3172=EDGE_CURVE('',#2666,#2667,#1573,.T.);
#3173=EDGE_CURVE('',#2667,#2662,#1574,.T.);
#3174=EDGE_CURVE('',#2668,#2668,#2394,.T.);
#3175=EDGE_CURVE('',#2669,#2670,#1575,.T.);
#3176=EDGE_CURVE('',#2670,#2662,#1576,.T.);
#3177=EDGE_CURVE('',#2669,#2667,#1577,.T.);
#3178=EDGE_CURVE('',#2671,#2669,#1578,.T.);
#3179=EDGE_CURVE('',#2671,#2666,#1579,.T.);
#3180=EDGE_CURVE('',#2672,#2671,#1580,.T.);
#3181=EDGE_CURVE('',#2672,#2665,#1581,.T.);
#3182=EDGE_CURVE('',#2673,#2672,#1582,.T.);
#3183=EDGE_CURVE('',#2673,#2664,#1583,.T.);
#3184=EDGE_CURVE('',#2674,#2673,#1584,.T.);
#3185=EDGE_CURVE('',#2674,#2663,#1585,.T.);
#3186=EDGE_CURVE('',#2670,#2674,#1586,.T.);
#3187=EDGE_CURVE('',#2675,#2675,#2395,.T.);
#3188=EDGE_CURVE('',#2675,#2668,#1587,.T.);
#3189=EDGE_CURVE('',#2676,#2676,#2396,.T.);
#3190=EDGE_CURVE('',#2676,#2677,#1588,.T.);
#3191=EDGE_CURVE('',#2677,#2677,#2397,.T.);
#3192=EDGE_CURVE('',#2678,#2678,#2398,.T.);
#3193=EDGE_CURVE('',#2679,#2679,#2399,.T.);
#3194=EDGE_CURVE('',#2679,#2678,#1589,.T.);
#3195=EDGE_CURVE('',#2680,#2680,#2400,.T.);
#3196=EDGE_CURVE('',#2680,#2681,#1590,.T.);
#3197=EDGE_CURVE('',#2681,#2681,#2401,.T.);
#3198=EDGE_CURVE('',#2682,#2682,#2402,.T.);
#3199=EDGE_CURVE('',#2683,#2683,#2403,.T.);
#3200=EDGE_CURVE('',#2683,#2682,#1591,.T.);
#3201=EDGE_CURVE('',#2684,#2684,#2404,.T.);
#3202=EDGE_CURVE('',#2684,#2685,#1592,.T.);
#3203=EDGE_CURVE('',#2685,#2685,#2405,.T.);
#3204=EDGE_CURVE('',#2686,#2686,#2406,.T.);
#3205=EDGE_CURVE('',#2686,#2687,#1593,.T.);
#3206=EDGE_CURVE('',#2687,#2687,#2407,.T.);
#3207=EDGE_CURVE('',#2688,#2689,#1594,.T.);
#3208=EDGE_CURVE('',#2689,#2690,#1595,.T.);
#3209=EDGE_CURVE('',#2691,#2690,#1596,.T.);
#3210=EDGE_CURVE('',#2688,#2691,#1597,.T.);
#3211=EDGE_CURVE('',#2692,#2688,#1598,.T.);
#3212=EDGE_CURVE('',#2693,#2691,#1599,.T.);
#3213=EDGE_CURVE('',#2692,#2693,#1600,.T.);
#3214=EDGE_CURVE('',#2694,#2692,#1601,.T.);
#3215=EDGE_CURVE('',#2695,#2693,#1602,.T.);
#3216=EDGE_CURVE('',#2694,#2695,#1603,.T.);
#3217=EDGE_CURVE('',#2689,#2694,#1604,.T.);
#3218=EDGE_CURVE('',#2690,#2695,#1605,.T.);
#3219=EDGE_CURVE('',#2696,#2696,#2408,.T.);
#3220=EDGE_CURVE('',#2696,#2697,#1606,.T.);
#3221=EDGE_CURVE('',#2697,#2697,#2409,.T.);
#3222=EDGE_CURVE('',#2698,#2698,#2410,.T.);
#3223=EDGE_CURVE('',#2699,#2699,#2411,.T.);
#3224=EDGE_CURVE('',#2699,#2698,#1607,.T.);
#3225=EDGE_CURVE('',#2700,#2700,#2412,.T.);
#3226=EDGE_CURVE('',#2700,#2701,#1608,.T.);
#3227=EDGE_CURVE('',#2701,#2701,#2413,.T.);
#3228=EDGE_CURVE('',#2702,#2702,#2414,.T.);
#3229=EDGE_CURVE('',#2703,#2703,#2415,.T.);
#3230=EDGE_CURVE('',#2703,#2702,#1609,.T.);
#3231=EDGE_CURVE('',#2704,#2704,#2416,.T.);
#3232=EDGE_CURVE('',#2704,#2705,#1610,.T.);
#3233=EDGE_CURVE('',#2705,#2705,#2417,.T.);
#3234=EDGE_CURVE('',#2706,#2706,#2418,.T.);
#3235=EDGE_CURVE('',#2706,#2707,#1611,.T.);
#3236=EDGE_CURVE('',#2707,#2707,#2419,.T.);
#3237=EDGE_CURVE('',#2708,#2709,#1612,.T.);
#3238=EDGE_CURVE('',#2709,#2710,#1613,.T.);
#3239=EDGE_CURVE('',#2711,#2710,#1614,.T.);
#3240=EDGE_CURVE('',#2708,#2711,#1615,.T.);
#3241=EDGE_CURVE('',#2712,#2708,#1616,.T.);
#3242=EDGE_CURVE('',#2713,#2711,#1617,.T.);
#3243=EDGE_CURVE('',#2712,#2713,#1618,.T.);
#3244=EDGE_CURVE('',#2714,#2712,#1619,.T.);
#3245=EDGE_CURVE('',#2715,#2713,#1620,.T.);
#3246=EDGE_CURVE('',#2714,#2715,#1621,.T.);
#3247=EDGE_CURVE('',#2709,#2714,#1622,.T.);
#3248=EDGE_CURVE('',#2710,#2715,#1623,.T.);
#3249=EDGE_CURVE('',#2716,#2716,#2420,.F.);
#3250=EDGE_CURVE('',#2716,#2717,#1624,.T.);
#3251=EDGE_CURVE('',#2717,#2717,#2421,.F.);
#3252=EDGE_CURVE('',#2718,#2718,#2422,.T.);
#3253=EDGE_CURVE('',#2718,#2716,#1625,.T.);
#3254=EDGE_CURVE('',#2719,#2719,#2423,.T.);
#3255=EDGE_CURVE('',#2719,#2720,#1626,.T.);
#3256=EDGE_CURVE('',#2721,#2720,#246,.T.);
#3257=EDGE_CURVE('',#2722,#2721,#247,.T.);
#3258=EDGE_CURVE('',#2723,#2722,#248,.T.);
#3259=EDGE_CURVE('',#2724,#2723,#249,.T.);
#3260=EDGE_CURVE('',#2725,#2724,#250,.T.);
#3261=EDGE_CURVE('',#2720,#2725,#251,.T.);
#3262=EDGE_CURVE('',#2726,#2724,#1627,.T.);
#3263=EDGE_CURVE('',#2726,#2727,#1628,.T.);
#3264=EDGE_CURVE('',#2727,#2725,#1629,.T.);
#3265=EDGE_CURVE('',#2728,#2723,#1630,.T.);
#3266=EDGE_CURVE('',#2728,#2726,#1631,.T.);
#3267=EDGE_CURVE('',#2729,#2722,#1632,.T.);
#3268=EDGE_CURVE('',#2729,#2728,#1633,.T.);
#3269=EDGE_CURVE('',#2730,#2721,#1634,.T.);
#3270=EDGE_CURVE('',#2730,#2729,#1635,.T.);
#3271=EDGE_CURVE('',#2731,#2720,#1636,.T.);
#3272=EDGE_CURVE('',#2731,#2730,#1637,.T.);
#3273=EDGE_CURVE('',#2727,#2731,#1638,.T.);
#3274=EDGE_CURVE('',#2732,#2732,#2424,.T.);
#3275=EDGE_CURVE('',#2732,#2733,#1639,.T.);
#3276=EDGE_CURVE('',#2733,#2733,#2425,.T.);
#3277=EDGE_CURVE('',#2734,#2734,#2426,.T.);
#3278=EDGE_CURVE('',#2734,#2735,#1640,.T.);
#3279=EDGE_CURVE('',#2735,#2735,#2427,.T.);
#3280=EDGE_CURVE('',#2736,#2736,#2428,.T.);
#3281=EDGE_CURVE('',#2736,#2737,#1641,.T.);
#3282=EDGE_CURVE('',#2737,#2737,#2429,.T.);
#3283=EDGE_CURVE('',#2738,#2738,#2430,.T.);
#3284=EDGE_CURVE('',#2738,#2739,#1642,.T.);
#3285=EDGE_CURVE('',#2739,#2739,#2431,.T.);
#3286=EDGE_CURVE('',#2740,#2740,#2432,.T.);
#3287=EDGE_CURVE('',#2740,#2741,#1643,.T.);
#3288=EDGE_CURVE('',#2741,#2741,#2433,.T.);
#3289=EDGE_CURVE('',#2742,#2742,#2434,.T.);
#3290=EDGE_CURVE('',#2742,#2743,#1644,.T.);
#3291=EDGE_CURVE('',#2743,#2743,#2435,.T.);
#3292=EDGE_CURVE('',#2744,#2745,#1645,.T.);
#3293=EDGE_CURVE('',#2746,#2744,#2436,.T.);
#3294=EDGE_CURVE('',#2747,#2746,#1646,.T.);
#3295=EDGE_CURVE('',#2745,#2747,#2437,.T.);
#3296=EDGE_CURVE('',#2748,#2744,#1647,.T.);
#3297=EDGE_CURVE('',#2749,#2748,#2438,.T.);
#3298=EDGE_CURVE('',#2746,#2749,#1648,.T.);
#3299=EDGE_CURVE('',#2747,#2750,#1649,.T.);
#3300=EDGE_CURVE('',#2750,#2751,#1650,.T.);
#3301=EDGE_CURVE('',#2751,#2752,#1651,.T.);
#3302=EDGE_CURVE('',#2752,#2753,#1652,.T.);
#3303=EDGE_CURVE('',#2753,#2745,#1653,.T.);
#3304=EDGE_CURVE('',#2754,#2754,#2439,.T.);
#3305=EDGE_CURVE('',#2754,#2755,#1654,.T.);
#3306=EDGE_CURVE('',#2755,#2755,#2440,.T.);
#3307=EDGE_CURVE('',#2756,#2756,#2441,.T.);
#3308=EDGE_CURVE('',#2756,#2757,#1655,.T.);
#3309=EDGE_CURVE('',#2757,#2757,#2442,.T.);
#3310=EDGE_CURVE('',#2758,#2758,#2443,.T.);
#3311=EDGE_CURVE('',#2749,#2748,#2444,.T.);
#3312=EDGE_CURVE('',#2759,#2753,#1656,.T.);
#3313=EDGE_CURVE('',#2759,#2760,#1657,.T.);
#3314=EDGE_CURVE('',#2760,#2750,#1658,.T.);
#3315=EDGE_CURVE('',#2761,#2759,#1659,.T.);
#3316=EDGE_CURVE('',#2761,#2752,#1660,.T.);
#3317=EDGE_CURVE('',#2762,#2761,#1661,.T.);
#3318=EDGE_CURVE('',#2762,#2751,#1662,.T.);
#3319=EDGE_CURVE('',#2760,#2762,#1663,.T.);
#3320=EDGE_CURVE('',#2763,#2763,#2445,.T.);
#3321=EDGE_CURVE('',#2763,#2764,#1664,.T.);
#3322=EDGE_CURVE('',#2764,#2764,#2446,.T.);
#3323=EDGE_CURVE('',#2765,#2765,#2447,.T.);
#3324=EDGE_CURVE('',#2765,#2766,#1665,.T.);
#3325=EDGE_CURVE('',#2766,#2766,#2448,.T.);
#3326=EDGE_CURVE('',#2767,#2767,#2449,.T.);
#3327=EDGE_CURVE('',#2767,#2768,#1666,.T.);
#3328=EDGE_CURVE('',#2768,#2768,#2450,.T.);
#3329=EDGE_CURVE('',#2769,#2769,#2451,.T.);
#3330=EDGE_CURVE('',#2769,#2770,#1667,.T.);
#3331=EDGE_CURVE('',#2770,#2770,#2452,.T.);
#3332=EDGE_CURVE('',#2771,#2771,#2453,.T.);
#3333=EDGE_CURVE('',#2771,#2772,#1668,.T.);
#3334=EDGE_CURVE('',#2772,#2772,#2454,.T.);
#3335=EDGE_CURVE('',#2773,#2773,#2455,.T.);
#3336=EDGE_CURVE('',#2773,#2774,#1669,.T.);
#3337=EDGE_CURVE('',#2774,#2774,#2456,.T.);
#3338=EDGE_CURVE('',#2775,#2776,#1670,.T.);
#3339=EDGE_CURVE('',#2777,#2775,#2457,.T.);
#3340=EDGE_CURVE('',#2778,#2777,#1671,.T.);
#3341=EDGE_CURVE('',#2776,#2778,#2458,.T.);
#3342=EDGE_CURVE('',#2779,#2775,#1672,.T.);
#3343=EDGE_CURVE('',#2780,#2779,#2459,.T.);
#3344=EDGE_CURVE('',#2777,#2780,#1673,.T.);
#3345=EDGE_CURVE('',#2778,#2781,#1674,.T.);
#3346=EDGE_CURVE('',#2781,#2782,#1675,.T.);
#3347=EDGE_CURVE('',#2782,#2783,#1676,.T.);
#3348=EDGE_CURVE('',#2783,#2784,#1677,.T.);
#3349=EDGE_CURVE('',#2784,#2776,#1678,.T.);
#3350=EDGE_CURVE('',#2785,#2785,#2460,.T.);
#3351=EDGE_CURVE('',#2785,#2786,#1679,.T.);
#3352=EDGE_CURVE('',#2786,#2786,#2461,.T.);
#3353=EDGE_CURVE('',#2787,#2787,#2462,.T.);
#3354=EDGE_CURVE('',#2787,#2788,#1680,.T.);
#3355=EDGE_CURVE('',#2788,#2788,#2463,.T.);
#3356=EDGE_CURVE('',#2789,#2789,#2464,.T.);
#3357=EDGE_CURVE('',#2780,#2779,#2465,.T.);
#3358=EDGE_CURVE('',#2790,#2791,#1681,.T.);
#3359=EDGE_CURVE('',#2791,#2783,#1682,.T.);
#3360=EDGE_CURVE('',#2790,#2782,#1683,.T.);
#3361=EDGE_CURVE('',#2792,#2790,#1684,.T.);
#3362=EDGE_CURVE('',#2792,#2781,#1685,.T.);
#3363=EDGE_CURVE('',#2793,#2784,#1686,.T.);
#3364=EDGE_CURVE('',#2793,#2792,#1687,.T.);
#3365=EDGE_CURVE('',#2791,#2793,#1688,.T.);
#3366=EDGE_CURVE('',#2794,#2794,#2466,.T.);
#3367=EDGE_CURVE('',#2794,#2795,#1689,.T.);
#3368=EDGE_CURVE('',#2795,#2795,#2467,.T.);
#3369=EDGE_CURVE('',#2796,#2796,#2468,.T.);
#3370=EDGE_CURVE('',#2796,#2797,#1690,.T.);
#3371=EDGE_CURVE('',#2797,#2797,#2469,.T.);
#3372=EDGE_CURVE('',#2798,#2798,#2470,.T.);
#3373=EDGE_CURVE('',#2798,#2799,#1691,.T.);
#3374=EDGE_CURVE('',#2799,#2799,#2471,.T.);
#3375=EDGE_CURVE('',#2800,#2800,#2472,.T.);
#3376=EDGE_CURVE('',#2800,#2801,#1692,.T.);
#3377=EDGE_CURVE('',#2801,#2801,#2473,.T.);
#3378=EDGE_CURVE('',#2802,#2803,#1693,.T.);
#3379=EDGE_CURVE('',#2802,#2804,#1694,.T.);
#3380=EDGE_CURVE('',#2805,#2804,#1695,.T.);
#3381=EDGE_CURVE('',#2803,#2805,#1696,.T.);
#3382=EDGE_CURVE('',#2806,#2807,#1697,.T.);
#3383=EDGE_CURVE('',#2806,#2808,#1698,.T.);
#3384=EDGE_CURVE('',#2809,#2808,#1699,.T.);
#3385=EDGE_CURVE('',#2807,#2809,#1700,.T.);
#3386=EDGE_CURVE('',#2810,#2802,#1701,.T.);
#3387=EDGE_CURVE('',#2811,#2810,#1702,.T.);
#3388=EDGE_CURVE('',#2804,#2811,#1703,.T.);
#3389=EDGE_CURVE('',#2812,#2806,#1704,.T.);
#3390=EDGE_CURVE('',#2813,#2812,#1705,.T.);
#3391=EDGE_CURVE('',#2808,#2813,#1706,.T.);
#3392=EDGE_CURVE('',#2811,#2809,#2474,.T.);
#3393=EDGE_CURVE('',#2813,#2814,#1707,.T.);
#3394=EDGE_CURVE('',#2814,#2815,#1708,.T.);
#3395=EDGE_CURVE('',#2815,#2816,#1709,.T.);
#3396=EDGE_CURVE('',#2816,#2817,#1710,.T.);
#3397=EDGE_CURVE('',#2817,#2805,#1711,.T.);
#3398=EDGE_CURVE('',#2818,#2812,#1712,.T.);
#3399=EDGE_CURVE('',#2818,#2814,#1713,.T.);
#3400=EDGE_CURVE('',#2819,#2817,#1714,.T.);
#3401=EDGE_CURVE('',#2803,#2819,#1715,.T.);
#3402=EDGE_CURVE('',#2807,#2810,#2475,.T.);
#3403=EDGE_CURVE('',#2819,#2820,#1716,.T.);
#3404=EDGE_CURVE('',#2820,#2816,#1717,.T.);
#3405=EDGE_CURVE('',#2820,#2821,#1718,.T.);
#3406=EDGE_CURVE('',#2821,#2815,#1719,.T.);
#3407=EDGE_CURVE('',#2821,#2818,#1720,.T.);
#3408=EDGE_CURVE('',#2822,#2822,#2476,.T.);
#3409=EDGE_CURVE('',#2823,#2823,#2477,.T.);
#3410=EDGE_CURVE('',#2824,#2824,#2478,.T.);
#3411=EDGE_CURVE('',#2824,#2822,#1721,.T.);
#3412=EDGE_CURVE('',#2825,#2825,#2479,.T.);
#3413=EDGE_CURVE('',#2825,#2826,#1722,.T.);
#3414=EDGE_CURVE('',#2826,#2826,#2480,.T.);
#3415=EDGE_CURVE('',#2823,#2827,#1723,.T.);
#3416=EDGE_CURVE('',#2827,#2827,#2481,.T.);
#3417=EDGE_CURVE('',#2828,#2828,#2482,.T.);
#3418=EDGE_CURVE('',#2828,#2828,#2483,.T.);
#3419=EDGE_CURVE('',#2829,#2829,#2484,.T.);
#3420=EDGE_CURVE('',#2829,#2830,#1724,.T.);
#3421=EDGE_CURVE('',#2830,#2830,#2485,.T.);
#3422=EDGE_CURVE('',#2831,#2831,#2486,.T.);
#3423=EDGE_CURVE('',#2832,#2832,#2487,.T.);
#3424=EDGE_CURVE('',#2832,#2831,#1725,.T.);
#3425=EDGE_CURVE('',#2833,#2833,#2488,.T.);
#3426=EDGE_CURVE('',#2833,#2834,#1726,.T.);
#3427=EDGE_CURVE('',#2834,#2834,#2489,.T.);
#3428=EDGE_CURVE('',#2835,#2835,#2490,.T.);
#3429=EDGE_CURVE('',#2835,#2836,#1727,.T.);
#3430=EDGE_CURVE('',#2836,#2836,#2491,.T.);
#3431=EDGE_CURVE('',#2837,#2837,#2492,.T.);
#3432=EDGE_CURVE('',#2837,#2838,#1728,.T.);
#3433=EDGE_CURVE('',#2838,#2838,#2493,.T.);
#3434=EDGE_CURVE('',#2839,#2839,#2494,.T.);
#3435=EDGE_CURVE('',#2839,#2840,#1729,.T.);
#3436=EDGE_CURVE('',#2840,#2840,#2495,.T.);
#3437=EDGE_CURVE('',#2841,#2841,#2496,.T.);
#3438=EDGE_CURVE('',#2841,#2842,#1730,.T.);
#3439=EDGE_CURVE('',#2842,#2842,#2497,.T.);
#3440=EDGE_CURVE('',#2843,#2843,#2498,.T.);
#3441=EDGE_CURVE('',#2843,#2844,#1731,.T.);
#3442=EDGE_CURVE('',#2844,#2844,#2499,.T.);
#3443=EDGE_CURVE('',#2845,#2845,#2500,.T.);
#3444=EDGE_CURVE('',#2845,#2846,#1732,.T.);
#3445=EDGE_CURVE('',#2846,#2846,#2501,.T.);
#3446=EDGE_CURVE('',#2847,#2847,#2502,.T.);
#3447=EDGE_CURVE('',#2847,#2848,#1733,.T.);
#3448=EDGE_CURVE('',#2848,#2848,#2503,.T.);
#3449=EDGE_CURVE('',#2849,#2850,#1734,.T.);
#3450=EDGE_CURVE('',#2850,#2851,#1735,.T.);
#3451=EDGE_CURVE('',#2852,#2851,#1736,.T.);
#3452=EDGE_CURVE('',#2849,#2852,#1737,.T.);
#3453=EDGE_CURVE('',#2853,#2849,#1738,.T.);
#3454=EDGE_CURVE('',#2854,#2852,#1739,.T.);
#3455=EDGE_CURVE('',#2853,#2854,#1740,.T.);
#3456=EDGE_CURVE('',#2855,#2853,#1741,.T.);
#3457=EDGE_CURVE('',#2856,#2854,#1742,.T.);
#3458=EDGE_CURVE('',#2855,#2856,#1743,.T.);
#3459=EDGE_CURVE('',#2850,#2855,#1744,.T.);
#3460=EDGE_CURVE('',#2851,#2856,#1745,.T.);
#3461=EDGE_CURVE('',#2857,#2857,#2504,.T.);
#3462=EDGE_CURVE('',#2858,#2858,#2505,.T.);
#3463=EDGE_CURVE('',#2858,#2859,#1746,.T.);
#3464=EDGE_CURVE('',#2859,#2859,#2506,.T.);
#3465=EDGE_CURVE('',#2860,#2860,#2507,.T.);
#3466=EDGE_CURVE('',#2860,#2861,#1747,.T.);
#3467=EDGE_CURVE('',#2861,#2861,#2508,.T.);
#3468=EDGE_CURVE('',#2862,#2863,#1748,.T.);
#3469=EDGE_CURVE('',#2863,#2864,#1749,.T.);
#3470=EDGE_CURVE('',#2864,#2865,#1750,.T.);
#3471=EDGE_CURVE('',#2862,#2865,#1751,.T.);
#3472=EDGE_CURVE('',#2863,#2866,#1752,.T.);
#3473=EDGE_CURVE('',#2866,#2867,#1753,.T.);
#3474=EDGE_CURVE('',#2867,#2864,#1754,.T.);
#3475=EDGE_CURVE('',#2866,#2868,#1755,.T.);
#3476=EDGE_CURVE('',#2868,#2869,#1756,.T.);
#3477=EDGE_CURVE('',#2869,#2867,#1757,.T.);
#3478=EDGE_CURVE('',#2868,#2870,#1758,.T.);
#3479=EDGE_CURVE('',#2870,#2871,#1759,.T.);
#3480=EDGE_CURVE('',#2871,#2869,#1760,.T.);
#3481=EDGE_CURVE('',#2870,#2872,#1761,.T.);
#3482=EDGE_CURVE('',#2872,#2873,#1762,.T.);
#3483=EDGE_CURVE('',#2873,#2871,#1763,.T.);
#3484=EDGE_CURVE('',#2872,#2862,#1764,.T.);
#3485=EDGE_CURVE('',#2865,#2873,#1765,.T.);
#3486=EDGE_CURVE('',#2874,#2874,#2509,.T.);
#3487=EDGE_CURVE('',#2875,#2875,#2510,.T.);
#3488=EDGE_CURVE('',#2874,#2876,#1766,.T.);
#3489=EDGE_CURVE('',#2876,#2876,#2511,.T.);
#3490=EDGE_CURVE('',#2877,#2877,#2512,.T.);
#3491=EDGE_CURVE('',#2878,#2878,#2513,.T.);
#3492=EDGE_CURVE('',#2878,#2877,#1767,.T.);
#3493=EDGE_CURVE('',#2879,#2879,#2514,.T.);
#3494=EDGE_CURVE('',#2879,#2878,#1768,.T.);
#3495=EDGE_CURVE('',#2880,#2880,#2515,.T.);
#3496=EDGE_CURVE('',#2880,#2879,#1769,.T.);
#3497=EDGE_CURVE('',#2881,#2881,#2516,.T.);
#3498=EDGE_CURVE('',#2882,#2882,#2517,.F.);
#3499=EDGE_CURVE('',#2882,#2881,#1770,.T.);
#3500=EDGE_CURVE('',#2875,#2882,#1771,.T.);
#3501=EDGE_CURVE('',#2883,#2883,#2518,.T.);
#3502=EDGE_CURVE('',#2883,#2884,#1772,.T.);
#3503=EDGE_CURVE('',#2884,#2884,#2519,.T.);
#3504=EDGE_CURVE('',#2884,#2885,#1773,.T.);
#3505=EDGE_CURVE('',#2885,#2885,#2520,.T.);
#3506=EDGE_CURVE('',#2886,#2886,#2521,.T.);
#3507=EDGE_CURVE('',#2886,#2887,#1774,.T.);
#3508=EDGE_CURVE('',#2887,#2887,#2522,.T.);
#3509=EDGE_CURVE('',#2888,#2889,#252,.T.);
#3510=EDGE_CURVE('',#2890,#2888,#253,.T.);
#3511=EDGE_CURVE('',#2890,#2891,#1775,.T.);
#3512=EDGE_CURVE('',#2891,#2891,#2523,.T.);
#3513=EDGE_CURVE('',#2892,#2890,#254,.T.);
#3514=EDGE_CURVE('',#2893,#2892,#255,.T.);
#3515=EDGE_CURVE('',#2894,#2893,#256,.T.);
#3516=EDGE_CURVE('',#2889,#2894,#257,.T.);
#3517=EDGE_CURVE('',#2895,#2895,#2524,.T.);
#3518=EDGE_CURVE('',#2895,#2896,#1776,.T.);
#3519=EDGE_CURVE('',#2897,#2896,#258,.T.);
#3520=EDGE_CURVE('',#2898,#2897,#259,.T.);
#3521=EDGE_CURVE('',#2899,#2898,#260,.T.);
#3522=EDGE_CURVE('',#2900,#2899,#261,.T.);
#3523=EDGE_CURVE('',#2901,#2900,#262,.T.);
#3524=EDGE_CURVE('',#2896,#2901,#263,.T.);
#3525=EDGE_CURVE('',#2892,#2901,#1777,.T.);
#3526=EDGE_CURVE('',#2893,#2900,#1778,.T.);
#3527=EDGE_CURVE('',#2890,#2896,#1779,.T.);
#3528=EDGE_CURVE('',#2888,#2897,#1780,.T.);
#3529=EDGE_CURVE('',#2902,#2902,#2525,.F.);
#3530=EDGE_CURVE('',#2902,#2903,#1781,.T.);
#3531=EDGE_CURVE('',#2903,#2903,#2526,.F.);
#3532=EDGE_CURVE('',#2889,#2898,#1782,.T.);
#3533=EDGE_CURVE('',#2894,#2899,#1783,.T.);
#3534=EDGE_CURVE('',#2904,#2905,#1784,.T.);
#3535=EDGE_CURVE('',#2905,#2906,#1785,.T.);
#3536=EDGE_CURVE('',#2906,#2907,#1786,.T.);
#3537=EDGE_CURVE('',#2907,#2908,#1787,.T.);
#3538=EDGE_CURVE('',#2908,#2909,#1788,.T.);
#3539=EDGE_CURVE('',#2909,#2904,#1789,.T.);
#3540=EDGE_CURVE('',#2910,#2910,#2527,.T.);
#3541=EDGE_CURVE('',#2911,#2912,#1790,.T.);
#3542=EDGE_CURVE('',#2912,#2913,#1791,.T.);
#3543=EDGE_CURVE('',#2913,#2914,#1792,.T.);
#3544=EDGE_CURVE('',#2914,#2915,#1793,.T.);
#3545=EDGE_CURVE('',#2915,#2916,#1794,.T.);
#3546=EDGE_CURVE('',#2916,#2911,#1795,.T.);
#3547=EDGE_CURVE('',#2917,#2917,#2528,.T.);
#3548=EDGE_CURVE('',#2911,#2905,#1796,.T.);
#3549=EDGE_CURVE('',#2906,#2916,#1797,.T.);
#3550=EDGE_CURVE('',#2907,#2915,#1798,.T.);
#3551=EDGE_CURVE('',#2908,#2914,#1799,.T.);
#3552=EDGE_CURVE('',#2909,#2913,#1800,.T.);
#3553=EDGE_CURVE('',#2904,#2912,#1801,.T.);
#3554=EDGE_CURVE('',#2917,#2918,#1802,.T.);
#3555=EDGE_CURVE('',#2918,#2918,#2529,.T.);
#3556=EDGE_CURVE('',#2919,#2919,#2530,.T.);
#3557=EDGE_CURVE('',#2920,#2920,#2531,.T.);
#3558=EDGE_CURVE('',#2918,#2919,#1803,.T.);
#3559=EDGE_CURVE('',#2921,#2921,#2532,.T.);
#3560=EDGE_CURVE('',#2921,#2910,#1804,.T.);
#3561=EDGE_CURVE('',#2922,#2922,#2533,.T.);
#3562=EDGE_CURVE('',#2922,#2921,#1805,.T.);
#3563=EDGE_CURVE('',#2923,#2923,#2534,.T.);
#3564=EDGE_CURVE('',#2923,#2920,#1806,.T.);
#3565=EDGE_CURVE('',#2924,#2924,#2535,.T.);
#3566=EDGE_CURVE('',#2924,#2925,#1807,.T.);
#3567=EDGE_CURVE('',#2925,#2925,#2536,.T.);
#3568=EDGE_CURVE('',#2926,#2926,#2537,.T.);
#3569=EDGE_CURVE('',#2926,#2927,#1808,.T.);
#3570=EDGE_CURVE('',#2927,#2927,#2538,.T.);
#3571=EDGE_CURVE('',#2928,#2928,#2539,.T.);
#3572=EDGE_CURVE('',#2929,#2929,#2540,.T.);
#3573=EDGE_CURVE('',#2929,#2928,#1809,.T.);
#3574=EDGE_CURVE('',#2930,#2930,#2541,.T.);
#3575=EDGE_CURVE('',#2930,#2929,#1810,.T.);
#3576=EDGE_CURVE('',#2931,#2931,#2542,.T.);
#3577=EDGE_CURVE('',#2931,#2930,#1811,.T.);
#3578=EDGE_CURVE('',#2932,#2932,#2543,.T.);
#3579=EDGE_CURVE('',#2933,#2933,#2544,.F.);
#3580=EDGE_CURVE('',#2933,#2932,#1812,.T.);
#3581=EDGE_CURVE('',#2934,#2934,#2545,.F.);
#3582=EDGE_CURVE('',#2934,#2933,#1813,.T.);
#3583=EDGE_CURVE('',#2935,#2935,#2546,.T.);
#3584=EDGE_CURVE('',#2935,#2934,#1814,.T.);
#3585=EDGE_CURVE('',#2936,#2937,#1815,.T.);
#3586=EDGE_CURVE('',#2937,#2938,#1816,.T.);
#3587=EDGE_CURVE('',#2938,#2939,#1817,.T.);
#3588=EDGE_CURVE('',#2936,#2939,#1818,.T.);
#3589=EDGE_CURVE('',#2937,#2940,#1819,.T.);
#3590=EDGE_CURVE('',#2940,#2941,#1820,.T.);
#3591=EDGE_CURVE('',#2941,#2938,#1821,.T.);
#3592=EDGE_CURVE('',#2940,#2942,#1822,.T.);
#3593=EDGE_CURVE('',#2942,#2943,#1823,.T.);
#3594=EDGE_CURVE('',#2943,#2941,#1824,.T.);
#3595=EDGE_CURVE('',#2942,#2944,#1825,.T.);
#3596=EDGE_CURVE('',#2944,#2945,#1826,.T.);
#3597=EDGE_CURVE('',#2945,#2943,#1827,.T.);
#3598=EDGE_CURVE('',#2944,#2946,#1828,.T.);
#3599=EDGE_CURVE('',#2946,#2947,#1829,.T.);
#3600=EDGE_CURVE('',#2947,#2945,#1830,.T.);
#3601=EDGE_CURVE('',#2946,#2936,#1831,.T.);
#3602=EDGE_CURVE('',#2939,#2947,#1832,.T.);
#3603=EDGE_CURVE('',#2948,#2948,#2547,.T.);
#3604=EDGE_CURVE('',#2948,#2949,#1833,.T.);
#3605=EDGE_CURVE('',#2949,#2949,#2548,.T.);
#3606=EDGE_CURVE('',#2950,#2951,#2549,.T.);
#3607=EDGE_CURVE('',#2952,#2950,#1834,.T.);
#3608=EDGE_CURVE('',#2953,#2952,#1835,.T.);
#3609=EDGE_CURVE('',#2953,#2951,#1836,.T.);
#3610=EDGE_CURVE('',#2951,#2954,#2550,.T.);
#3611=EDGE_CURVE('',#2955,#2953,#1837,.T.);
#3612=EDGE_CURVE('',#2955,#2956,#1838,.T.);
#3613=EDGE_CURVE('',#2954,#2956,#2551,.T.);
#3614=EDGE_CURVE('',#2956,#2957,#2552,.T.);
#3615=EDGE_CURVE('',#2958,#2955,#1839,.T.);
#3616=EDGE_CURVE('',#2958,#2957,#1840,.T.);
#3617=EDGE_CURVE('',#2957,#2950,#2553,.T.);
#3618=EDGE_CURVE('',#2952,#2958,#1841,.T.);
#3619=EDGE_CURVE('',#2959,#2959,#2554,.T.);
#3620=EDGE_CURVE('',#2959,#2960,#1842,.T.);
#3621=EDGE_CURVE('',#2960,#2960,#2555,.T.);
#3622=EDGE_CURVE('',#2954,#2961,#2556,.T.);
#3623=EDGE_CURVE('',#2962,#2962,#2557,.T.);
#3624=EDGE_CURVE('',#2962,#2963,#1843,.T.);
#3625=EDGE_CURVE('',#2963,#2963,#2558,.T.);
#3626=EDGE_CURVE('',#2964,#2965,#2559,.T.);
#3627=EDGE_CURVE('',#2966,#2965,#1844,.T.);
#3628=EDGE_CURVE('',#2964,#2966,#1845,.T.);
#3629=EDGE_CURVE('',#2967,#2968,#2560,.T.);
#3630=EDGE_CURVE('',#2969,#2968,#1846,.T.);
#3631=EDGE_CURVE('',#2967,#2969,#1847,.T.);
#3632=EDGE_CURVE('',#2970,#2971,#2561,.T.);
#3633=EDGE_CURVE('',#2972,#2971,#1848,.T.);
#3634=EDGE_CURVE('',#2970,#2972,#1849,.T.);
#3635=EDGE_CURVE('',#2973,#2974,#2562,.T.);
#3636=EDGE_CURVE('',#2975,#2974,#1850,.T.);
#3637=EDGE_CURVE('',#2973,#2975,#1851,.T.);
#3638=EDGE_CURVE('',#2964,#2974,#1852,.T.);
#3639=EDGE_CURVE('',#2966,#2976,#1853,.T.);
#3640=EDGE_CURVE('',#2977,#2976,#1854,.T.);
#3641=EDGE_CURVE('',#2975,#2977,#1855,.T.);
#3642=EDGE_CURVE('',#2973,#2971,#1856,.T.);
#3643=EDGE_CURVE('',#2978,#2977,#1857,.T.);
#3644=EDGE_CURVE('',#2972,#2978,#1858,.T.);
#3645=EDGE_CURVE('',#2970,#2968,#1859,.T.);
#3646=EDGE_CURVE('',#2979,#2978,#1860,.T.);
#3647=EDGE_CURVE('',#2969,#2979,#1861,.T.);
#3648=EDGE_CURVE('',#2967,#2965,#1862,.T.);
#3649=EDGE_CURVE('',#2976,#2979,#1863,.T.);
#3650=EDGE_CURVE('',#2968,#2970,#2563,.T.);
#3651=EDGE_CURVE('',#2965,#2980,#2564,.T.);
#3652=EDGE_CURVE('',#2980,#2967,#2565,.T.);
#3653=EDGE_CURVE('',#2974,#2964,#2566,.T.);
#3654=EDGE_CURVE('',#2971,#2973,#2567,.T.);
#3655=EDGE_CURVE('',#2981,#2982,#1864,.T.);
#3656=EDGE_CURVE('',#2982,#2983,#1865,.T.);
#3657=EDGE_CURVE('',#2984,#2983,#1866,.T.);
#3658=EDGE_CURVE('',#2981,#2984,#1867,.T.);
#3659=EDGE_CURVE('',#2985,#2981,#1868,.T.);
#3660=EDGE_CURVE('',#2986,#2984,#1869,.T.);
#3661=EDGE_CURVE('',#2985,#2986,#1870,.T.);
#3662=EDGE_CURVE('',#2987,#2985,#1871,.T.);
#3663=EDGE_CURVE('',#2988,#2986,#1872,.T.);
#3664=EDGE_CURVE('',#2987,#2988,#1873,.T.);
#3665=EDGE_CURVE('',#2982,#2987,#1874,.T.);
#3666=EDGE_CURVE('',#2983,#2988,#1875,.T.);
#3667=EDGE_CURVE('',#2980,#2989,#1876,.T.);
#3668=EDGE_CURVE('',#2989,#2989,#2568,.T.);
#3669=EDGE_CURVE('',#2990,#2991,#1877,.T.);
#3670=EDGE_CURVE('',#2992,#2990,#1878,.T.);
#3671=EDGE_CURVE('',#2993,#2992,#1879,.T.);
#3672=EDGE_CURVE('',#2993,#2991,#1880,.T.);
#3673=EDGE_CURVE('',#2991,#2994,#1881,.T.);
#3674=EDGE_CURVE('',#2995,#2993,#1882,.T.);
#3675=EDGE_CURVE('',#2995,#2994,#1883,.T.);
#3676=EDGE_CURVE('',#2994,#2996,#1884,.T.);
#3677=EDGE_CURVE('',#2997,#2995,#1885,.T.);
#3678=EDGE_CURVE('',#2997,#2996,#1886,.T.);
#3679=EDGE_CURVE('',#2996,#2990,#1887,.T.);
#3680=EDGE_CURVE('',#2992,#2997,#1888,.T.);
#3681=EDGE_CURVE('',#2998,#2999,#1889,.T.);
#3682=EDGE_CURVE('',#2999,#3000,#1890,.T.);
#3683=EDGE_CURVE('',#3001,#3000,#1891,.T.);
#3684=EDGE_CURVE('',#2998,#3001,#1892,.T.);
#3685=EDGE_CURVE('',#3002,#2998,#1893,.T.);
#3686=EDGE_CURVE('',#3003,#3001,#1894,.T.);
#3687=EDGE_CURVE('',#3002,#3003,#1895,.T.);
#3688=EDGE_CURVE('',#3004,#3002,#1896,.T.);
#3689=EDGE_CURVE('',#3005,#3003,#1897,.T.);
#3690=EDGE_CURVE('',#3004,#3005,#1898,.T.);
#3691=EDGE_CURVE('',#2999,#3004,#1899,.T.);
#3692=EDGE_CURVE('',#3000,#3005,#1900,.T.);
#3693=EDGE_CURVE('',#3006,#3006,#2569,.T.);
#3694=EDGE_CURVE('',#3006,#3007,#1901,.T.);
#3695=EDGE_CURVE('',#3007,#3007,#2570,.T.);
#3696=EDGE_CURVE('',#3008,#3008,#2571,.T.);
#3697=EDGE_CURVE('',#3008,#3009,#1902,.T.);
#3698=EDGE_CURVE('',#3009,#3009,#2572,.T.);
#3699=EDGE_CURVE('',#3010,#3011,#1903,.T.);
#3700=EDGE_CURVE('',#3011,#3012,#1904,.T.);
#3701=EDGE_CURVE('',#3013,#3012,#1905,.T.);
#3702=EDGE_CURVE('',#3010,#3013,#1906,.T.);
#3703=EDGE_CURVE('',#3014,#3010,#1907,.T.);
#3704=EDGE_CURVE('',#3015,#3013,#1908,.T.);
#3705=EDGE_CURVE('',#3014,#3015,#1909,.T.);
#3706=EDGE_CURVE('',#3016,#3014,#1910,.T.);
#3707=EDGE_CURVE('',#3017,#3015,#1911,.T.);
#3708=EDGE_CURVE('',#3016,#3017,#1912,.T.);
#3709=EDGE_CURVE('',#3011,#3016,#1913,.T.);
#3710=EDGE_CURVE('',#3012,#3017,#1914,.T.);
#3711=EDGE_CURVE('',#3018,#3019,#1915,.T.);
#3712=EDGE_CURVE('',#3019,#3020,#1916,.T.);
#3713=EDGE_CURVE('',#3020,#3021,#1917,.T.);
#3714=EDGE_CURVE('',#3018,#3021,#1918,.T.);
#3715=EDGE_CURVE('',#3019,#3022,#1919,.T.);
#3716=EDGE_CURVE('',#3022,#3023,#1920,.T.);
#3717=EDGE_CURVE('',#3023,#3020,#1921,.T.);
#3718=EDGE_CURVE('',#3022,#3024,#1922,.T.);
#3719=EDGE_CURVE('',#3024,#3025,#1923,.T.);
#3720=EDGE_CURVE('',#3025,#3023,#1924,.T.);
#3721=EDGE_CURVE('',#3024,#3026,#1925,.T.);
#3722=EDGE_CURVE('',#3026,#3027,#1926,.T.);
#3723=EDGE_CURVE('',#3027,#3025,#1927,.T.);
#3724=EDGE_CURVE('',#3026,#3028,#1928,.T.);
#3725=EDGE_CURVE('',#3028,#3029,#1929,.T.);
#3726=EDGE_CURVE('',#3029,#3027,#1930,.T.);
#3727=EDGE_CURVE('',#3028,#3018,#1931,.T.);
#3728=EDGE_CURVE('',#3021,#3029,#1932,.T.);
#3729=EDGE_CURVE('',#3030,#3030,#2573,.T.);
#3730=EDGE_CURVE('',#3031,#3031,#2574,.T.);
#3731=EDGE_CURVE('',#3032,#3032,#2575,.T.);
#3732=EDGE_CURVE('',#3032,#3031,#1933,.T.);
#3733=EDGE_CURVE('',#3033,#3033,#2576,.T.);
#3734=EDGE_CURVE('',#3033,#3032,#1934,.T.);
#3735=EDGE_CURVE('',#3034,#3034,#2577,.T.);
#3736=EDGE_CURVE('',#3034,#3033,#1935,.T.);
#3737=EDGE_CURVE('',#3035,#3035,#2578,.T.);
#3738=EDGE_CURVE('',#3036,#3036,#2579,.F.);
#3739=EDGE_CURVE('',#3036,#3035,#1936,.T.);
#3740=EDGE_CURVE('',#3030,#3036,#1937,.T.);
#3741=ORIENTED_EDGE('',*,*,#3037,.F.);
#3742=ORIENTED_EDGE('',*,*,#3038,.T.);
#3743=ORIENTED_EDGE('',*,*,#3039,.T.);
#3744=ORIENTED_EDGE('',*,*,#3038,.F.);
#3745=ORIENTED_EDGE('',*,*,#3039,.F.);
#3746=ORIENTED_EDGE('',*,*,#3040,.F.);
#3747=ORIENTED_EDGE('',*,*,#3041,.T.);
#3748=ORIENTED_EDGE('',*,*,#3042,.T.);
#3749=ORIENTED_EDGE('',*,*,#3041,.F.);
#3750=ORIENTED_EDGE('',*,*,#3042,.F.);
#3751=ORIENTED_EDGE('',*,*,#3043,.F.);
#3752=ORIENTED_EDGE('',*,*,#3044,.T.);
#3753=ORIENTED_EDGE('',*,*,#3045,.F.);
#3754=ORIENTED_EDGE('',*,*,#3044,.F.);
#3755=ORIENTED_EDGE('',*,*,#3043,.T.);
#3756=ORIENTED_EDGE('',*,*,#3046,.F.);
#3757=ORIENTED_EDGE('',*,*,#3047,.F.);
#3758=ORIENTED_EDGE('',*,*,#3048,.T.);
#3759=ORIENTED_EDGE('',*,*,#3049,.T.);
#3760=ORIENTED_EDGE('',*,*,#3048,.F.);
#3761=ORIENTED_EDGE('',*,*,#3049,.F.);
#3762=ORIENTED_EDGE('',*,*,#3050,.F.);
#3763=ORIENTED_EDGE('',*,*,#3051,.F.);
#3764=ORIENTED_EDGE('',*,*,#3052,.F.);
#3765=ORIENTED_EDGE('',*,*,#3053,.F.);
#3766=ORIENTED_EDGE('',*,*,#3052,.T.);
#3767=ORIENTED_EDGE('',*,*,#3054,.F.);
#3768=ORIENTED_EDGE('',*,*,#3055,.F.);
#3769=ORIENTED_EDGE('',*,*,#3056,.T.);
#3770=ORIENTED_EDGE('',*,*,#3057,.F.);
#3771=ORIENTED_EDGE('',*,*,#3058,.F.);
#3772=ORIENTED_EDGE('',*,*,#3059,.F.);
#3773=ORIENTED_EDGE('',*,*,#3060,.F.);
#3774=ORIENTED_EDGE('',*,*,#3061,.F.);
#3775=ORIENTED_EDGE('',*,*,#3062,.F.);
#3776=ORIENTED_EDGE('',*,*,#3063,.F.);
#3777=ORIENTED_EDGE('',*,*,#3064,.F.);
#3778=ORIENTED_EDGE('',*,*,#3056,.F.);
#3779=ORIENTED_EDGE('',*,*,#3050,.T.);
#3780=ORIENTED_EDGE('',*,*,#3065,.T.);
#3781=ORIENTED_EDGE('',*,*,#3066,.T.);
#3782=ORIENTED_EDGE('',*,*,#3067,.T.);
#3783=ORIENTED_EDGE('',*,*,#3068,.T.);
#3784=ORIENTED_EDGE('',*,*,#3069,.T.);
#3785=ORIENTED_EDGE('',*,*,#3070,.T.);
#3786=ORIENTED_EDGE('',*,*,#3071,.T.);
#3787=ORIENTED_EDGE('',*,*,#3072,.T.);
#3788=ORIENTED_EDGE('',*,*,#3073,.T.);
#3789=ORIENTED_EDGE('',*,*,#3074,.T.);
#3790=ORIENTED_EDGE('',*,*,#3075,.T.);
#3791=ORIENTED_EDGE('',*,*,#3076,.T.);
#3792=ORIENTED_EDGE('',*,*,#3077,.T.);
#3793=ORIENTED_EDGE('',*,*,#3078,.T.);
#3794=ORIENTED_EDGE('',*,*,#3079,.T.);
#3795=ORIENTED_EDGE('',*,*,#3080,.T.);
#3796=ORIENTED_EDGE('',*,*,#3081,.T.);
#3797=ORIENTED_EDGE('',*,*,#3082,.T.);
#3798=ORIENTED_EDGE('',*,*,#3083,.T.);
#3799=ORIENTED_EDGE('',*,*,#3084,.T.);
#3800=ORIENTED_EDGE('',*,*,#3085,.T.);
#3801=ORIENTED_EDGE('',*,*,#3086,.T.);
#3802=ORIENTED_EDGE('',*,*,#3087,.T.);
#3803=ORIENTED_EDGE('',*,*,#3088,.T.);
#3804=ORIENTED_EDGE('',*,*,#3089,.T.);
#3805=ORIENTED_EDGE('',*,*,#3090,.T.);
#3806=ORIENTED_EDGE('',*,*,#3091,.T.);
#3807=ORIENTED_EDGE('',*,*,#3092,.T.);
#3808=ORIENTED_EDGE('',*,*,#3093,.T.);
#3809=ORIENTED_EDGE('',*,*,#3094,.T.);
#3810=ORIENTED_EDGE('',*,*,#3095,.T.);
#3811=ORIENTED_EDGE('',*,*,#3096,.T.);
#3812=ORIENTED_EDGE('',*,*,#3097,.T.);
#3813=ORIENTED_EDGE('',*,*,#3098,.T.);
#3814=ORIENTED_EDGE('',*,*,#3099,.T.);
#3815=ORIENTED_EDGE('',*,*,#3100,.T.);
#3816=ORIENTED_EDGE('',*,*,#3101,.T.);
#3817=ORIENTED_EDGE('',*,*,#3102,.T.);
#3818=ORIENTED_EDGE('',*,*,#3103,.T.);
#3819=ORIENTED_EDGE('',*,*,#3104,.T.);
#3820=ORIENTED_EDGE('',*,*,#3105,.T.);
#3821=ORIENTED_EDGE('',*,*,#3106,.T.);
#3822=ORIENTED_EDGE('',*,*,#3107,.T.);
#3823=ORIENTED_EDGE('',*,*,#3108,.T.);
#3824=ORIENTED_EDGE('',*,*,#3109,.T.);
#3825=ORIENTED_EDGE('',*,*,#3110,.T.);
#3826=ORIENTED_EDGE('',*,*,#3061,.T.);
#3827=ORIENTED_EDGE('',*,*,#3111,.T.);
#3828=ORIENTED_EDGE('',*,*,#3112,.T.);
#3829=ORIENTED_EDGE('',*,*,#3113,.T.);
#3830=ORIENTED_EDGE('',*,*,#3114,.T.);
#3831=ORIENTED_EDGE('',*,*,#3059,.T.);
#3832=ORIENTED_EDGE('',*,*,#3054,.T.);
#3833=ORIENTED_EDGE('',*,*,#3051,.T.);
#3834=ORIENTED_EDGE('',*,*,#3053,.T.);
#3835=ORIENTED_EDGE('',*,*,#3058,.T.);
#3836=ORIENTED_EDGE('',*,*,#3115,.T.);
#3837=ORIENTED_EDGE('',*,*,#3116,.T.);
#3838=ORIENTED_EDGE('',*,*,#3117,.T.);
#3839=ORIENTED_EDGE('',*,*,#3062,.T.);
#3840=ORIENTED_EDGE('',*,*,#3118,.T.);
#3841=ORIENTED_EDGE('',*,*,#3046,.T.);
#3842=ORIENTED_EDGE('',*,*,#3118,.F.);
#3843=ORIENTED_EDGE('',*,*,#3057,.T.);
#3844=ORIENTED_EDGE('',*,*,#3064,.T.);
#3845=ORIENTED_EDGE('',*,*,#3055,.T.);
#3846=ORIENTED_EDGE('',*,*,#3110,.F.);
#3847=ORIENTED_EDGE('',*,*,#3119,.T.);
#3848=ORIENTED_EDGE('',*,*,#3120,.T.);
#3849=ORIENTED_EDGE('',*,*,#3121,.T.);
#3850=ORIENTED_EDGE('',*,*,#3095,.F.);
#3851=ORIENTED_EDGE('',*,*,#3122,.T.);
#3852=ORIENTED_EDGE('',*,*,#3123,.T.);
#3853=ORIENTED_EDGE('',*,*,#3124,.T.);
#3854=ORIENTED_EDGE('',*,*,#3080,.F.);
#3855=ORIENTED_EDGE('',*,*,#3125,.T.);
#3856=ORIENTED_EDGE('',*,*,#3126,.T.);
#3857=ORIENTED_EDGE('',*,*,#3127,.T.);
#3858=ORIENTED_EDGE('',*,*,#3065,.F.);
#3859=ORIENTED_EDGE('',*,*,#3063,.T.);
#3860=ORIENTED_EDGE('',*,*,#3117,.F.);
#3861=ORIENTED_EDGE('',*,*,#3128,.F.);
#3862=ORIENTED_EDGE('',*,*,#3111,.F.);
#3863=ORIENTED_EDGE('',*,*,#3129,.F.);
#3864=ORIENTED_EDGE('',*,*,#3130,.T.);
#3865=ORIENTED_EDGE('',*,*,#3112,.F.);
#3866=ORIENTED_EDGE('',*,*,#3128,.T.);
#3867=ORIENTED_EDGE('',*,*,#3116,.F.);
#3868=ORIENTED_EDGE('',*,*,#3131,.T.);
#3869=ORIENTED_EDGE('',*,*,#3113,.F.);
#3870=ORIENTED_EDGE('',*,*,#3130,.F.);
#3871=ORIENTED_EDGE('',*,*,#3060,.T.);
#3872=ORIENTED_EDGE('',*,*,#3114,.F.);
#3873=ORIENTED_EDGE('',*,*,#3131,.F.);
#3874=ORIENTED_EDGE('',*,*,#3115,.F.);
#3875=ORIENTED_EDGE('',*,*,#3103,.F.);
#3876=ORIENTED_EDGE('',*,*,#3132,.F.);
#3877=ORIENTED_EDGE('',*,*,#3104,.F.);
#3878=ORIENTED_EDGE('',*,*,#3132,.T.);
#3879=ORIENTED_EDGE('',*,*,#3102,.F.);
#3880=ORIENTED_EDGE('',*,*,#3121,.F.);
#3881=ORIENTED_EDGE('',*,*,#3133,.T.);
#3882=ORIENTED_EDGE('',*,*,#3119,.F.);
#3883=ORIENTED_EDGE('',*,*,#3105,.F.);
#3884=ORIENTED_EDGE('',*,*,#3101,.F.);
#3885=ORIENTED_EDGE('',*,*,#3134,.F.);
#3886=ORIENTED_EDGE('',*,*,#3096,.F.);
#3887=ORIENTED_EDGE('',*,*,#3109,.F.);
#3888=ORIENTED_EDGE('',*,*,#3135,.F.);
#3889=ORIENTED_EDGE('',*,*,#3120,.F.);
#3890=ORIENTED_EDGE('',*,*,#3133,.F.);
#3891=ORIENTED_EDGE('',*,*,#3135,.T.);
#3892=ORIENTED_EDGE('',*,*,#3108,.F.);
#3893=ORIENTED_EDGE('',*,*,#3136,.F.);
#3894=ORIENTED_EDGE('',*,*,#3097,.F.);
#3895=ORIENTED_EDGE('',*,*,#3137,.F.);
#3896=ORIENTED_EDGE('',*,*,#3138,.T.);
#3897=ORIENTED_EDGE('',*,*,#3098,.F.);
#3898=ORIENTED_EDGE('',*,*,#3136,.T.);
#3899=ORIENTED_EDGE('',*,*,#3107,.F.);
#3900=ORIENTED_EDGE('',*,*,#3139,.T.);
#3901=ORIENTED_EDGE('',*,*,#3099,.F.);
#3902=ORIENTED_EDGE('',*,*,#3138,.F.);
#3903=ORIENTED_EDGE('',*,*,#3134,.T.);
#3904=ORIENTED_EDGE('',*,*,#3100,.F.);
#3905=ORIENTED_EDGE('',*,*,#3139,.F.);
#3906=ORIENTED_EDGE('',*,*,#3106,.F.);
#3907=ORIENTED_EDGE('',*,*,#3088,.F.);
#3908=ORIENTED_EDGE('',*,*,#3140,.F.);
#3909=ORIENTED_EDGE('',*,*,#3089,.F.);
#3910=ORIENTED_EDGE('',*,*,#3140,.T.);
#3911=ORIENTED_EDGE('',*,*,#3087,.F.);
#3912=ORIENTED_EDGE('',*,*,#3124,.F.);
#3913=ORIENTED_EDGE('',*,*,#3141,.T.);
#3914=ORIENTED_EDGE('',*,*,#3122,.F.);
#3915=ORIENTED_EDGE('',*,*,#3090,.F.);
#3916=ORIENTED_EDGE('',*,*,#3086,.F.);
#3917=ORIENTED_EDGE('',*,*,#3142,.F.);
#3918=ORIENTED_EDGE('',*,*,#3081,.F.);
#3919=ORIENTED_EDGE('',*,*,#3094,.F.);
#3920=ORIENTED_EDGE('',*,*,#3143,.F.);
#3921=ORIENTED_EDGE('',*,*,#3123,.F.);
#3922=ORIENTED_EDGE('',*,*,#3141,.F.);
#3923=ORIENTED_EDGE('',*,*,#3143,.T.);
#3924=ORIENTED_EDGE('',*,*,#3093,.F.);
#3925=ORIENTED_EDGE('',*,*,#3144,.F.);
#3926=ORIENTED_EDGE('',*,*,#3082,.F.);
#3927=ORIENTED_EDGE('',*,*,#3145,.F.);
#3928=ORIENTED_EDGE('',*,*,#3146,.T.);
#3929=ORIENTED_EDGE('',*,*,#3083,.F.);
#3930=ORIENTED_EDGE('',*,*,#3144,.T.);
#3931=ORIENTED_EDGE('',*,*,#3092,.F.);
#3932=ORIENTED_EDGE('',*,*,#3147,.T.);
#3933=ORIENTED_EDGE('',*,*,#3084,.F.);
#3934=ORIENTED_EDGE('',*,*,#3146,.F.);
#3935=ORIENTED_EDGE('',*,*,#3142,.T.);
#3936=ORIENTED_EDGE('',*,*,#3085,.F.);
#3937=ORIENTED_EDGE('',*,*,#3147,.F.);
#3938=ORIENTED_EDGE('',*,*,#3091,.F.);
#3939=ORIENTED_EDGE('',*,*,#3073,.F.);
#3940=ORIENTED_EDGE('',*,*,#3148,.F.);
#3941=ORIENTED_EDGE('',*,*,#3074,.F.);
#3942=ORIENTED_EDGE('',*,*,#3148,.T.);
#3943=ORIENTED_EDGE('',*,*,#3072,.F.);
#3944=ORIENTED_EDGE('',*,*,#3127,.F.);
#3945=ORIENTED_EDGE('',*,*,#3149,.T.);
#3946=ORIENTED_EDGE('',*,*,#3125,.F.);
#3947=ORIENTED_EDGE('',*,*,#3075,.F.);
#3948=ORIENTED_EDGE('',*,*,#3071,.F.);
#3949=ORIENTED_EDGE('',*,*,#3150,.F.);
#3950=ORIENTED_EDGE('',*,*,#3066,.F.);
#3951=ORIENTED_EDGE('',*,*,#3079,.F.);
#3952=ORIENTED_EDGE('',*,*,#3151,.F.);
#3953=ORIENTED_EDGE('',*,*,#3126,.F.);
#3954=ORIENTED_EDGE('',*,*,#3149,.F.);
#3955=ORIENTED_EDGE('',*,*,#3151,.T.);
#3956=ORIENTED_EDGE('',*,*,#3078,.F.);
#3957=ORIENTED_EDGE('',*,*,#3152,.F.);
#3958=ORIENTED_EDGE('',*,*,#3067,.F.);
#3959=ORIENTED_EDGE('',*,*,#3153,.F.);
#3960=ORIENTED_EDGE('',*,*,#3154,.T.);
#3961=ORIENTED_EDGE('',*,*,#3068,.F.);
#3962=ORIENTED_EDGE('',*,*,#3152,.T.);
#3963=ORIENTED_EDGE('',*,*,#3077,.F.);
#3964=ORIENTED_EDGE('',*,*,#3155,.T.);
#3965=ORIENTED_EDGE('',*,*,#3069,.F.);
#3966=ORIENTED_EDGE('',*,*,#3154,.F.);
#3967=ORIENTED_EDGE('',*,*,#3150,.T.);
#3968=ORIENTED_EDGE('',*,*,#3070,.F.);
#3969=ORIENTED_EDGE('',*,*,#3155,.F.);
#3970=ORIENTED_EDGE('',*,*,#3076,.F.);
#3971=ORIENTED_EDGE('',*,*,#3156,.T.);
#3972=ORIENTED_EDGE('',*,*,#3157,.T.);
#3973=ORIENTED_EDGE('',*,*,#3158,.F.);
#3974=ORIENTED_EDGE('',*,*,#3159,.F.);
#3975=ORIENTED_EDGE('',*,*,#3160,.T.);
#3976=ORIENTED_EDGE('',*,*,#3159,.T.);
#3977=ORIENTED_EDGE('',*,*,#3161,.F.);
#3978=ORIENTED_EDGE('',*,*,#3162,.F.);
#3979=ORIENTED_EDGE('',*,*,#3045,.T.);
#3980=ORIENTED_EDGE('',*,*,#3163,.T.);
#3981=ORIENTED_EDGE('',*,*,#3162,.T.);
#3982=ORIENTED_EDGE('',*,*,#3164,.F.);
#3983=ORIENTED_EDGE('',*,*,#3165,.F.);
#3984=ORIENTED_EDGE('',*,*,#3129,.T.);
#3985=ORIENTED_EDGE('',*,*,#3137,.T.);
#3986=ORIENTED_EDGE('',*,*,#3145,.T.);
#3987=ORIENTED_EDGE('',*,*,#3153,.T.);
#3988=ORIENTED_EDGE('',*,*,#3166,.T.);
#3989=ORIENTED_EDGE('',*,*,#3165,.T.);
#3990=ORIENTED_EDGE('',*,*,#3167,.F.);
#3991=ORIENTED_EDGE('',*,*,#3157,.F.);
#3992=ORIENTED_EDGE('',*,*,#3047,.T.);
#3993=ORIENTED_EDGE('',*,*,#3167,.T.);
#3994=ORIENTED_EDGE('',*,*,#3164,.T.);
#3995=ORIENTED_EDGE('',*,*,#3161,.T.);
#3996=ORIENTED_EDGE('',*,*,#3158,.T.);
#3997=ORIENTED_EDGE('',*,*,#3166,.F.);
#3998=ORIENTED_EDGE('',*,*,#3156,.F.);
#3999=ORIENTED_EDGE('',*,*,#3160,.F.);
#4000=ORIENTED_EDGE('',*,*,#3163,.F.);
#4001=ORIENTED_EDGE('',*,*,#3037,.T.);
#4002=ORIENTED_EDGE('',*,*,#3040,.T.);
#4003=ORIENTED_EDGE('',*,*,#3168,.T.);
#4004=ORIENTED_EDGE('',*,*,#3169,.T.);
#4005=ORIENTED_EDGE('',*,*,#3170,.T.);
#4006=ORIENTED_EDGE('',*,*,#3171,.T.);
#4007=ORIENTED_EDGE('',*,*,#3172,.T.);
#4008=ORIENTED_EDGE('',*,*,#3173,.T.);
#4009=ORIENTED_EDGE('',*,*,#3174,.F.);
#4010=ORIENTED_EDGE('',*,*,#3175,.T.);
#4011=ORIENTED_EDGE('',*,*,#3176,.T.);
#4012=ORIENTED_EDGE('',*,*,#3173,.F.);
#4013=ORIENTED_EDGE('',*,*,#3177,.F.);
#4014=ORIENTED_EDGE('',*,*,#3178,.T.);
#4015=ORIENTED_EDGE('',*,*,#3177,.T.);
#4016=ORIENTED_EDGE('',*,*,#3172,.F.);
#4017=ORIENTED_EDGE('',*,*,#3179,.F.);
#4018=ORIENTED_EDGE('',*,*,#3180,.T.);
#4019=ORIENTED_EDGE('',*,*,#3179,.T.);
#4020=ORIENTED_EDGE('',*,*,#3171,.F.);
#4021=ORIENTED_EDGE('',*,*,#3181,.F.);
#4022=ORIENTED_EDGE('',*,*,#3182,.T.);
#4023=ORIENTED_EDGE('',*,*,#3181,.T.);
#4024=ORIENTED_EDGE('',*,*,#3170,.F.);
#4025=ORIENTED_EDGE('',*,*,#3183,.F.);
#4026=ORIENTED_EDGE('',*,*,#3184,.T.);
#4027=ORIENTED_EDGE('',*,*,#3183,.T.);
#4028=ORIENTED_EDGE('',*,*,#3169,.F.);
#4029=ORIENTED_EDGE('',*,*,#3185,.F.);
#4030=ORIENTED_EDGE('',*,*,#3186,.T.);
#4031=ORIENTED_EDGE('',*,*,#3185,.T.);
#4032=ORIENTED_EDGE('',*,*,#3168,.F.);
#4033=ORIENTED_EDGE('',*,*,#3176,.F.);
#4034=ORIENTED_EDGE('',*,*,#3186,.F.);
#4035=ORIENTED_EDGE('',*,*,#3175,.F.);
#4036=ORIENTED_EDGE('',*,*,#3178,.F.);
#4037=ORIENTED_EDGE('',*,*,#3180,.F.);
#4038=ORIENTED_EDGE('',*,*,#3182,.F.);
#4039=ORIENTED_EDGE('',*,*,#3184,.F.);
#4040=ORIENTED_EDGE('',*,*,#3187,.F.);
#4041=ORIENTED_EDGE('',*,*,#3188,.T.);
#4042=ORIENTED_EDGE('',*,*,#3174,.T.);
#4043=ORIENTED_EDGE('',*,*,#3188,.F.);
#4044=ORIENTED_EDGE('',*,*,#3187,.T.);
#4045=ORIENTED_EDGE('',*,*,#3189,.F.);
#4046=ORIENTED_EDGE('',*,*,#3190,.T.);
#4047=ORIENTED_EDGE('',*,*,#3191,.F.);
#4048=ORIENTED_EDGE('',*,*,#3190,.F.);
#4049=ORIENTED_EDGE('',*,*,#3189,.T.);
#4050=ORIENTED_EDGE('',*,*,#3192,.F.);
#4051=ORIENTED_EDGE('',*,*,#3193,.F.);
#4052=ORIENTED_EDGE('',*,*,#3194,.T.);
#4053=ORIENTED_EDGE('',*,*,#3192,.T.);
#4054=ORIENTED_EDGE('',*,*,#3194,.F.);
#4055=ORIENTED_EDGE('',*,*,#3195,.F.);
#4056=ORIENTED_EDGE('',*,*,#3196,.T.);
#4057=ORIENTED_EDGE('',*,*,#3197,.F.);
#4058=ORIENTED_EDGE('',*,*,#3196,.F.);
#4059=ORIENTED_EDGE('',*,*,#3195,.T.);
#4060=ORIENTED_EDGE('',*,*,#3198,.F.);
#4061=ORIENTED_EDGE('',*,*,#3199,.F.);
#4062=ORIENTED_EDGE('',*,*,#3200,.T.);
#4063=ORIENTED_EDGE('',*,*,#3198,.T.);
#4064=ORIENTED_EDGE('',*,*,#3200,.F.);
#4065=ORIENTED_EDGE('',*,*,#3201,.F.);
#4066=ORIENTED_EDGE('',*,*,#3202,.T.);
#4067=ORIENTED_EDGE('',*,*,#3203,.T.);
#4068=ORIENTED_EDGE('',*,*,#3202,.F.);
#4069=ORIENTED_EDGE('',*,*,#3203,.F.);
#4070=ORIENTED_EDGE('',*,*,#3204,.F.);
#4071=ORIENTED_EDGE('',*,*,#3204,.T.);
#4072=ORIENTED_EDGE('',*,*,#3205,.T.);
#4073=ORIENTED_EDGE('',*,*,#3206,.F.);
#4074=ORIENTED_EDGE('',*,*,#3205,.F.);
#4075=ORIENTED_EDGE('',*,*,#3207,.T.);
#4076=ORIENTED_EDGE('',*,*,#3208,.T.);
#4077=ORIENTED_EDGE('',*,*,#3209,.F.);
#4078=ORIENTED_EDGE('',*,*,#3210,.F.);
#4079=ORIENTED_EDGE('',*,*,#3211,.T.);
#4080=ORIENTED_EDGE('',*,*,#3210,.T.);
#4081=ORIENTED_EDGE('',*,*,#3212,.F.);
#4082=ORIENTED_EDGE('',*,*,#3213,.F.);
#4083=ORIENTED_EDGE('',*,*,#3214,.T.);
#4084=ORIENTED_EDGE('',*,*,#3213,.T.);
#4085=ORIENTED_EDGE('',*,*,#3215,.F.);
#4086=ORIENTED_EDGE('',*,*,#3216,.F.);
#4087=ORIENTED_EDGE('',*,*,#3217,.T.);
#4088=ORIENTED_EDGE('',*,*,#3216,.T.);
#4089=ORIENTED_EDGE('',*,*,#3218,.F.);
#4090=ORIENTED_EDGE('',*,*,#3208,.F.);
#4091=ORIENTED_EDGE('',*,*,#3218,.T.);
#4092=ORIENTED_EDGE('',*,*,#3215,.T.);
#4093=ORIENTED_EDGE('',*,*,#3212,.T.);
#4094=ORIENTED_EDGE('',*,*,#3209,.T.);
#4095=ORIENTED_EDGE('',*,*,#3191,.T.);
#4096=ORIENTED_EDGE('',*,*,#3197,.T.);
#4097=ORIENTED_EDGE('',*,*,#3206,.T.);
#4098=ORIENTED_EDGE('',*,*,#3217,.F.);
#4099=ORIENTED_EDGE('',*,*,#3207,.F.);
#4100=ORIENTED_EDGE('',*,*,#3211,.F.);
#4101=ORIENTED_EDGE('',*,*,#3214,.F.);
#4102=ORIENTED_EDGE('',*,*,#3193,.T.);
#4103=ORIENTED_EDGE('',*,*,#3199,.T.);
#4104=ORIENTED_EDGE('',*,*,#3201,.T.);
#4105=ORIENTED_EDGE('',*,*,#3219,.F.);
#4106=ORIENTED_EDGE('',*,*,#3220,.T.);
#4107=ORIENTED_EDGE('',*,*,#3221,.F.);
#4108=ORIENTED_EDGE('',*,*,#3220,.F.);
#4109=ORIENTED_EDGE('',*,*,#3219,.T.);
#4110=ORIENTED_EDGE('',*,*,#3222,.F.);
#4111=ORIENTED_EDGE('',*,*,#3223,.F.);
#4112=ORIENTED_EDGE('',*,*,#3224,.T.);
#4113=ORIENTED_EDGE('',*,*,#3222,.T.);
#4114=ORIENTED_EDGE('',*,*,#3224,.F.);
#4115=ORIENTED_EDGE('',*,*,#3225,.F.);
#4116=ORIENTED_EDGE('',*,*,#3226,.T.);
#4117=ORIENTED_EDGE('',*,*,#3227,.F.);
#4118=ORIENTED_EDGE('',*,*,#3226,.F.);
#4119=ORIENTED_EDGE('',*,*,#3225,.T.);
#4120=ORIENTED_EDGE('',*,*,#3228,.F.);
#4121=ORIENTED_EDGE('',*,*,#3229,.F.);
#4122=ORIENTED_EDGE('',*,*,#3230,.T.);
#4123=ORIENTED_EDGE('',*,*,#3228,.T.);
#4124=ORIENTED_EDGE('',*,*,#3230,.F.);
#4125=ORIENTED_EDGE('',*,*,#3231,.F.);
#4126=ORIENTED_EDGE('',*,*,#3232,.T.);
#4127=ORIENTED_EDGE('',*,*,#3233,.T.);
#4128=ORIENTED_EDGE('',*,*,#3232,.F.);
#4129=ORIENTED_EDGE('',*,*,#3233,.F.);
#4130=ORIENTED_EDGE('',*,*,#3234,.F.);
#4131=ORIENTED_EDGE('',*,*,#3234,.T.);
#4132=ORIENTED_EDGE('',*,*,#3235,.T.);
#4133=ORIENTED_EDGE('',*,*,#3236,.F.);
#4134=ORIENTED_EDGE('',*,*,#3235,.F.);
#4135=ORIENTED_EDGE('',*,*,#3237,.T.);
#4136=ORIENTED_EDGE('',*,*,#3238,.T.);
#4137=ORIENTED_EDGE('',*,*,#3239,.F.);
#4138=ORIENTED_EDGE('',*,*,#3240,.F.);
#4139=ORIENTED_EDGE('',*,*,#3241,.T.);
#4140=ORIENTED_EDGE('',*,*,#3240,.T.);
#4141=ORIENTED_EDGE('',*,*,#3242,.F.);
#4142=ORIENTED_EDGE('',*,*,#3243,.F.);
#4143=ORIENTED_EDGE('',*,*,#3244,.T.);
#4144=ORIENTED_EDGE('',*,*,#3243,.T.);
#4145=ORIENTED_EDGE('',*,*,#3245,.F.);
#4146=ORIENTED_EDGE('',*,*,#3246,.F.);
#4147=ORIENTED_EDGE('',*,*,#3247,.T.);
#4148=ORIENTED_EDGE('',*,*,#3246,.T.);
#4149=ORIENTED_EDGE('',*,*,#3248,.F.);
#4150=ORIENTED_EDGE('',*,*,#3238,.F.);
#4151=ORIENTED_EDGE('',*,*,#3248,.T.);
#4152=ORIENTED_EDGE('',*,*,#3245,.T.);
#4153=ORIENTED_EDGE('',*,*,#3242,.T.);
#4154=ORIENTED_EDGE('',*,*,#3239,.T.);
#4155=ORIENTED_EDGE('',*,*,#3221,.T.);
#4156=ORIENTED_EDGE('',*,*,#3227,.T.);
#4157=ORIENTED_EDGE('',*,*,#3236,.T.);
#4158=ORIENTED_EDGE('',*,*,#3247,.F.);
#4159=ORIENTED_EDGE('',*,*,#3237,.F.);
#4160=ORIENTED_EDGE('',*,*,#3241,.F.);
#4161=ORIENTED_EDGE('',*,*,#3244,.F.);
#4162=ORIENTED_EDGE('',*,*,#3223,.T.);
#4163=ORIENTED_EDGE('',*,*,#3229,.T.);
#4164=ORIENTED_EDGE('',*,*,#3231,.T.);
#4165=ORIENTED_EDGE('',*,*,#3249,.F.);
#4166=ORIENTED_EDGE('',*,*,#3250,.T.);
#4167=ORIENTED_EDGE('',*,*,#3251,.F.);
#4168=ORIENTED_EDGE('',*,*,#3250,.F.);
#4169=ORIENTED_EDGE('',*,*,#3252,.F.);
#4170=ORIENTED_EDGE('',*,*,#3253,.T.);
#4171=ORIENTED_EDGE('',*,*,#3249,.T.);
#4172=ORIENTED_EDGE('',*,*,#3253,.F.);
#4173=ORIENTED_EDGE('',*,*,#3252,.T.);
#4174=ORIENTED_EDGE('',*,*,#3254,.F.);
#4175=ORIENTED_EDGE('',*,*,#3255,.T.);
#4176=ORIENTED_EDGE('',*,*,#3256,.F.);
#4177=ORIENTED_EDGE('',*,*,#3257,.F.);
#4178=ORIENTED_EDGE('',*,*,#3258,.F.);
#4179=ORIENTED_EDGE('',*,*,#3259,.F.);
#4180=ORIENTED_EDGE('',*,*,#3260,.F.);
#4181=ORIENTED_EDGE('',*,*,#3261,.F.);
#4182=ORIENTED_EDGE('',*,*,#3255,.F.);
#4183=ORIENTED_EDGE('',*,*,#3260,.T.);
#4184=ORIENTED_EDGE('',*,*,#3262,.F.);
#4185=ORIENTED_EDGE('',*,*,#3263,.T.);
#4186=ORIENTED_EDGE('',*,*,#3264,.T.);
#4187=ORIENTED_EDGE('',*,*,#3259,.T.);
#4188=ORIENTED_EDGE('',*,*,#3265,.F.);
#4189=ORIENTED_EDGE('',*,*,#3266,.T.);
#4190=ORIENTED_EDGE('',*,*,#3262,.T.);
#4191=ORIENTED_EDGE('',*,*,#3258,.T.);
#4192=ORIENTED_EDGE('',*,*,#3267,.F.);
#4193=ORIENTED_EDGE('',*,*,#3268,.T.);
#4194=ORIENTED_EDGE('',*,*,#3265,.T.);
#4195=ORIENTED_EDGE('',*,*,#3257,.T.);
#4196=ORIENTED_EDGE('',*,*,#3269,.F.);
#4197=ORIENTED_EDGE('',*,*,#3270,.T.);
#4198=ORIENTED_EDGE('',*,*,#3267,.T.);
#4199=ORIENTED_EDGE('',*,*,#3256,.T.);
#4200=ORIENTED_EDGE('',*,*,#3271,.F.);
#4201=ORIENTED_EDGE('',*,*,#3272,.T.);
#4202=ORIENTED_EDGE('',*,*,#3269,.T.);
#4203=ORIENTED_EDGE('',*,*,#3261,.T.);
#4204=ORIENTED_EDGE('',*,*,#3264,.F.);
#4205=ORIENTED_EDGE('',*,*,#3273,.T.);
#4206=ORIENTED_EDGE('',*,*,#3271,.T.);
#4207=ORIENTED_EDGE('',*,*,#3254,.T.);
#4208=ORIENTED_EDGE('',*,*,#3268,.F.);
#4209=ORIENTED_EDGE('',*,*,#3270,.F.);
#4210=ORIENTED_EDGE('',*,*,#3272,.F.);
#4211=ORIENTED_EDGE('',*,*,#3273,.F.);
#4212=ORIENTED_EDGE('',*,*,#3263,.F.);
#4213=ORIENTED_EDGE('',*,*,#3266,.F.);
#4214=ORIENTED_EDGE('',*,*,#3251,.T.);
#4215=ORIENTED_EDGE('',*,*,#3274,.F.);
#4216=ORIENTED_EDGE('',*,*,#3275,.T.);
#4217=ORIENTED_EDGE('',*,*,#3276,.F.);
#4218=ORIENTED_EDGE('',*,*,#3275,.F.);
#4219=ORIENTED_EDGE('',*,*,#3274,.T.);
#4220=ORIENTED_EDGE('',*,*,#3277,.F.);
#4221=ORIENTED_EDGE('',*,*,#3278,.T.);
#4222=ORIENTED_EDGE('',*,*,#3279,.F.);
#4223=ORIENTED_EDGE('',*,*,#3278,.F.);
#4224=ORIENTED_EDGE('',*,*,#3277,.T.);
#4225=ORIENTED_EDGE('',*,*,#3280,.F.);
#4226=ORIENTED_EDGE('',*,*,#3281,.T.);
#4227=ORIENTED_EDGE('',*,*,#3282,.F.);
#4228=ORIENTED_EDGE('',*,*,#3281,.F.);
#4229=ORIENTED_EDGE('',*,*,#3283,.F.);
#4230=ORIENTED_EDGE('',*,*,#3284,.T.);
#4231=ORIENTED_EDGE('',*,*,#3285,.F.);
#4232=ORIENTED_EDGE('',*,*,#3284,.F.);
#4233=ORIENTED_EDGE('',*,*,#3286,.F.);
#4234=ORIENTED_EDGE('',*,*,#3287,.T.);
#4235=ORIENTED_EDGE('',*,*,#3288,.F.);
#4236=ORIENTED_EDGE('',*,*,#3287,.F.);
#4237=ORIENTED_EDGE('',*,*,#3289,.F.);
#4238=ORIENTED_EDGE('',*,*,#3290,.T.);
#4239=ORIENTED_EDGE('',*,*,#3291,.F.);
#4240=ORIENTED_EDGE('',*,*,#3290,.F.);
#4241=ORIENTED_EDGE('',*,*,#3292,.F.);
#4242=ORIENTED_EDGE('',*,*,#3293,.F.);
#4243=ORIENTED_EDGE('',*,*,#3294,.F.);
#4244=ORIENTED_EDGE('',*,*,#3295,.F.);
#4245=ORIENTED_EDGE('',*,*,#3296,.F.);
#4246=ORIENTED_EDGE('',*,*,#3297,.F.);
#4247=ORIENTED_EDGE('',*,*,#3298,.F.);
#4248=ORIENTED_EDGE('',*,*,#3293,.T.);
#4249=ORIENTED_EDGE('',*,*,#3295,.T.);
#4250=ORIENTED_EDGE('',*,*,#3299,.T.);
#4251=ORIENTED_EDGE('',*,*,#3300,.T.);
#4252=ORIENTED_EDGE('',*,*,#3301,.T.);
#4253=ORIENTED_EDGE('',*,*,#3302,.T.);
#4254=ORIENTED_EDGE('',*,*,#3303,.T.);
#4255=ORIENTED_EDGE('',*,*,#3276,.T.);
#4256=ORIENTED_EDGE('',*,*,#3279,.T.);
#4257=ORIENTED_EDGE('',*,*,#3304,.F.);
#4258=ORIENTED_EDGE('',*,*,#3305,.T.);
#4259=ORIENTED_EDGE('',*,*,#3306,.F.);
#4260=ORIENTED_EDGE('',*,*,#3305,.F.);
#4261=ORIENTED_EDGE('',*,*,#3307,.F.);
#4262=ORIENTED_EDGE('',*,*,#3308,.T.);
#4263=ORIENTED_EDGE('',*,*,#3309,.T.);
#4264=ORIENTED_EDGE('',*,*,#3308,.F.);
#4265=ORIENTED_EDGE('',*,*,#3309,.F.);
#4266=ORIENTED_EDGE('',*,*,#3310,.F.);
#4267=ORIENTED_EDGE('',*,*,#3307,.T.);
#4268=ORIENTED_EDGE('',*,*,#3306,.T.);
#4269=ORIENTED_EDGE('',*,*,#3297,.T.);
#4270=ORIENTED_EDGE('',*,*,#3311,.F.);
#4271=ORIENTED_EDGE('',*,*,#3310,.T.);
#4272=ORIENTED_EDGE('',*,*,#3292,.T.);
#4273=ORIENTED_EDGE('',*,*,#3303,.F.);
#4274=ORIENTED_EDGE('',*,*,#3312,.F.);
#4275=ORIENTED_EDGE('',*,*,#3313,.T.);
#4276=ORIENTED_EDGE('',*,*,#3314,.T.);
#4277=ORIENTED_EDGE('',*,*,#3299,.F.);
#4278=ORIENTED_EDGE('',*,*,#3294,.T.);
#4279=ORIENTED_EDGE('',*,*,#3298,.T.);
#4280=ORIENTED_EDGE('',*,*,#3311,.T.);
#4281=ORIENTED_EDGE('',*,*,#3296,.T.);
#4282=ORIENTED_EDGE('',*,*,#3282,.T.);
#4283=ORIENTED_EDGE('',*,*,#3285,.T.);
#4284=ORIENTED_EDGE('',*,*,#3288,.T.);
#4285=ORIENTED_EDGE('',*,*,#3291,.T.);
#4286=ORIENTED_EDGE('',*,*,#3315,.T.);
#4287=ORIENTED_EDGE('',*,*,#3312,.T.);
#4288=ORIENTED_EDGE('',*,*,#3302,.F.);
#4289=ORIENTED_EDGE('',*,*,#3316,.F.);
#4290=ORIENTED_EDGE('',*,*,#3317,.T.);
#4291=ORIENTED_EDGE('',*,*,#3316,.T.);
#4292=ORIENTED_EDGE('',*,*,#3301,.F.);
#4293=ORIENTED_EDGE('',*,*,#3318,.F.);
#4294=ORIENTED_EDGE('',*,*,#3304,.T.);
#4295=ORIENTED_EDGE('',*,*,#3289,.T.);
#4296=ORIENTED_EDGE('',*,*,#3286,.T.);
#4297=ORIENTED_EDGE('',*,*,#3283,.T.);
#4298=ORIENTED_EDGE('',*,*,#3280,.T.);
#4299=ORIENTED_EDGE('',*,*,#3319,.T.);
#4300=ORIENTED_EDGE('',*,*,#3318,.T.);
#4301=ORIENTED_EDGE('',*,*,#3300,.F.);
#4302=ORIENTED_EDGE('',*,*,#3314,.F.);
#4303=ORIENTED_EDGE('',*,*,#3319,.F.);
#4304=ORIENTED_EDGE('',*,*,#3313,.F.);
#4305=ORIENTED_EDGE('',*,*,#3315,.F.);
#4306=ORIENTED_EDGE('',*,*,#3317,.F.);
#4307=ORIENTED_EDGE('',*,*,#3320,.F.);
#4308=ORIENTED_EDGE('',*,*,#3321,.T.);
#4309=ORIENTED_EDGE('',*,*,#3322,.F.);
#4310=ORIENTED_EDGE('',*,*,#3321,.F.);
#4311=ORIENTED_EDGE('',*,*,#3320,.T.);
#4312=ORIENTED_EDGE('',*,*,#3323,.F.);
#4313=ORIENTED_EDGE('',*,*,#3324,.T.);
#4314=ORIENTED_EDGE('',*,*,#3325,.F.);
#4315=ORIENTED_EDGE('',*,*,#3324,.F.);
#4316=ORIENTED_EDGE('',*,*,#3323,.T.);
#4317=ORIENTED_EDGE('',*,*,#3326,.F.);
#4318=ORIENTED_EDGE('',*,*,#3327,.T.);
#4319=ORIENTED_EDGE('',*,*,#3328,.F.);
#4320=ORIENTED_EDGE('',*,*,#3327,.F.);
#4321=ORIENTED_EDGE('',*,*,#3329,.F.);
#4322=ORIENTED_EDGE('',*,*,#3330,.T.);
#4323=ORIENTED_EDGE('',*,*,#3331,.F.);
#4324=ORIENTED_EDGE('',*,*,#3330,.F.);
#4325=ORIENTED_EDGE('',*,*,#3332,.F.);
#4326=ORIENTED_EDGE('',*,*,#3333,.T.);
#4327=ORIENTED_EDGE('',*,*,#3334,.F.);
#4328=ORIENTED_EDGE('',*,*,#3333,.F.);
#4329=ORIENTED_EDGE('',*,*,#3335,.F.);
#4330=ORIENTED_EDGE('',*,*,#3336,.T.);
#4331=ORIENTED_EDGE('',*,*,#3337,.F.);
#4332=ORIENTED_EDGE('',*,*,#3336,.F.);
#4333=ORIENTED_EDGE('',*,*,#3338,.F.);
#4334=ORIENTED_EDGE('',*,*,#3339,.F.);
#4335=ORIENTED_EDGE('',*,*,#3340,.F.);
#4336=ORIENTED_EDGE('',*,*,#3341,.F.);
#4337=ORIENTED_EDGE('',*,*,#3342,.F.);
#4338=ORIENTED_EDGE('',*,*,#3343,.F.);
#4339=ORIENTED_EDGE('',*,*,#3344,.F.);
#4340=ORIENTED_EDGE('',*,*,#3339,.T.);
#4341=ORIENTED_EDGE('',*,*,#3341,.T.);
#4342=ORIENTED_EDGE('',*,*,#3345,.T.);
#4343=ORIENTED_EDGE('',*,*,#3346,.T.);
#4344=ORIENTED_EDGE('',*,*,#3347,.T.);
#4345=ORIENTED_EDGE('',*,*,#3348,.T.);
#4346=ORIENTED_EDGE('',*,*,#3349,.T.);
#4347=ORIENTED_EDGE('',*,*,#3322,.T.);
#4348=ORIENTED_EDGE('',*,*,#3325,.T.);
#4349=ORIENTED_EDGE('',*,*,#3350,.F.);
#4350=ORIENTED_EDGE('',*,*,#3351,.T.);
#4351=ORIENTED_EDGE('',*,*,#3352,.F.);
#4352=ORIENTED_EDGE('',*,*,#3351,.F.);
#4353=ORIENTED_EDGE('',*,*,#3353,.F.);
#4354=ORIENTED_EDGE('',*,*,#3354,.T.);
#4355=ORIENTED_EDGE('',*,*,#3355,.T.);
#4356=ORIENTED_EDGE('',*,*,#3354,.F.);
#4357=ORIENTED_EDGE('',*,*,#3355,.F.);
#4358=ORIENTED_EDGE('',*,*,#3350,.T.);
#4359=ORIENTED_EDGE('',*,*,#3353,.T.);
#4360=ORIENTED_EDGE('',*,*,#3356,.F.);
#4361=ORIENTED_EDGE('',*,*,#3343,.T.);
#4362=ORIENTED_EDGE('',*,*,#3357,.F.);
#4363=ORIENTED_EDGE('',*,*,#3356,.T.);
#4364=ORIENTED_EDGE('',*,*,#3358,.T.);
#4365=ORIENTED_EDGE('',*,*,#3359,.T.);
#4366=ORIENTED_EDGE('',*,*,#3347,.F.);
#4367=ORIENTED_EDGE('',*,*,#3360,.F.);
#4368=ORIENTED_EDGE('',*,*,#3352,.T.);
#4369=ORIENTED_EDGE('',*,*,#3337,.T.);
#4370=ORIENTED_EDGE('',*,*,#3334,.T.);
#4371=ORIENTED_EDGE('',*,*,#3331,.T.);
#4372=ORIENTED_EDGE('',*,*,#3328,.T.);
#4373=ORIENTED_EDGE('',*,*,#3361,.T.);
#4374=ORIENTED_EDGE('',*,*,#3360,.T.);
#4375=ORIENTED_EDGE('',*,*,#3346,.F.);
#4376=ORIENTED_EDGE('',*,*,#3362,.F.);
#4377=ORIENTED_EDGE('',*,*,#3338,.T.);
#4378=ORIENTED_EDGE('',*,*,#3349,.F.);
#4379=ORIENTED_EDGE('',*,*,#3363,.F.);
#4380=ORIENTED_EDGE('',*,*,#3364,.T.);
#4381=ORIENTED_EDGE('',*,*,#3362,.T.);
#4382=ORIENTED_EDGE('',*,*,#3345,.F.);
#4383=ORIENTED_EDGE('',*,*,#3340,.T.);
#4384=ORIENTED_EDGE('',*,*,#3344,.T.);
#4385=ORIENTED_EDGE('',*,*,#3357,.T.);
#4386=ORIENTED_EDGE('',*,*,#3342,.T.);
#4387=ORIENTED_EDGE('',*,*,#3326,.T.);
#4388=ORIENTED_EDGE('',*,*,#3329,.T.);
#4389=ORIENTED_EDGE('',*,*,#3332,.T.);
#4390=ORIENTED_EDGE('',*,*,#3335,.T.);
#4391=ORIENTED_EDGE('',*,*,#3365,.T.);
#4392=ORIENTED_EDGE('',*,*,#3363,.T.);
#4393=ORIENTED_EDGE('',*,*,#3348,.F.);
#4394=ORIENTED_EDGE('',*,*,#3359,.F.);
#4395=ORIENTED_EDGE('',*,*,#3365,.F.);
#4396=ORIENTED_EDGE('',*,*,#3358,.F.);
#4397=ORIENTED_EDGE('',*,*,#3361,.F.);
#4398=ORIENTED_EDGE('',*,*,#3364,.F.);
#4399=ORIENTED_EDGE('',*,*,#3366,.F.);
#4400=ORIENTED_EDGE('',*,*,#3367,.T.);
#4401=ORIENTED_EDGE('',*,*,#3368,.F.);
#4402=ORIENTED_EDGE('',*,*,#3367,.F.);
#4403=ORIENTED_EDGE('',*,*,#3369,.F.);
#4404=ORIENTED_EDGE('',*,*,#3370,.T.);
#4405=ORIENTED_EDGE('',*,*,#3371,.F.);
#4406=ORIENTED_EDGE('',*,*,#3370,.F.);
#4407=ORIENTED_EDGE('',*,*,#3372,.F.);
#4408=ORIENTED_EDGE('',*,*,#3373,.T.);
#4409=ORIENTED_EDGE('',*,*,#3374,.F.);
#4410=ORIENTED_EDGE('',*,*,#3373,.F.);
#4411=ORIENTED_EDGE('',*,*,#3375,.F.);
#4412=ORIENTED_EDGE('',*,*,#3376,.T.);
#4413=ORIENTED_EDGE('',*,*,#3377,.F.);
#4414=ORIENTED_EDGE('',*,*,#3376,.F.);
#4415=ORIENTED_EDGE('',*,*,#3378,.F.);
#4416=ORIENTED_EDGE('',*,*,#3379,.T.);
#4417=ORIENTED_EDGE('',*,*,#3380,.F.);
#4418=ORIENTED_EDGE('',*,*,#3381,.F.);
#4419=ORIENTED_EDGE('',*,*,#3382,.F.);
#4420=ORIENTED_EDGE('',*,*,#3383,.T.);
#4421=ORIENTED_EDGE('',*,*,#3384,.F.);
#4422=ORIENTED_EDGE('',*,*,#3385,.F.);
#4423=ORIENTED_EDGE('',*,*,#3386,.F.);
#4424=ORIENTED_EDGE('',*,*,#3387,.F.);
#4425=ORIENTED_EDGE('',*,*,#3388,.F.);
#4426=ORIENTED_EDGE('',*,*,#3379,.F.);
#4427=ORIENTED_EDGE('',*,*,#3389,.F.);
#4428=ORIENTED_EDGE('',*,*,#3390,.F.);
#4429=ORIENTED_EDGE('',*,*,#3391,.F.);
#4430=ORIENTED_EDGE('',*,*,#3383,.F.);
#4431=ORIENTED_EDGE('',*,*,#3380,.T.);
#4432=ORIENTED_EDGE('',*,*,#3388,.T.);
#4433=ORIENTED_EDGE('',*,*,#3392,.T.);
#4434=ORIENTED_EDGE('',*,*,#3384,.T.);
#4435=ORIENTED_EDGE('',*,*,#3391,.T.);
#4436=ORIENTED_EDGE('',*,*,#3393,.T.);
#4437=ORIENTED_EDGE('',*,*,#3394,.T.);
#4438=ORIENTED_EDGE('',*,*,#3395,.T.);
#4439=ORIENTED_EDGE('',*,*,#3396,.T.);
#4440=ORIENTED_EDGE('',*,*,#3397,.T.);
#4441=ORIENTED_EDGE('',*,*,#3368,.T.);
#4442=ORIENTED_EDGE('',*,*,#3371,.T.);
#4443=ORIENTED_EDGE('',*,*,#3374,.T.);
#4444=ORIENTED_EDGE('',*,*,#3377,.T.);
#4445=ORIENTED_EDGE('',*,*,#3390,.T.);
#4446=ORIENTED_EDGE('',*,*,#3398,.F.);
#4447=ORIENTED_EDGE('',*,*,#3399,.T.);
#4448=ORIENTED_EDGE('',*,*,#3393,.F.);
#4449=ORIENTED_EDGE('',*,*,#3381,.T.);
#4450=ORIENTED_EDGE('',*,*,#3397,.F.);
#4451=ORIENTED_EDGE('',*,*,#3400,.F.);
#4452=ORIENTED_EDGE('',*,*,#3401,.F.);
#4453=ORIENTED_EDGE('',*,*,#3387,.T.);
#4454=ORIENTED_EDGE('',*,*,#3402,.F.);
#4455=ORIENTED_EDGE('',*,*,#3385,.T.);
#4456=ORIENTED_EDGE('',*,*,#3392,.F.);
#4457=ORIENTED_EDGE('',*,*,#3403,.F.);
#4458=ORIENTED_EDGE('',*,*,#3400,.T.);
#4459=ORIENTED_EDGE('',*,*,#3396,.F.);
#4460=ORIENTED_EDGE('',*,*,#3404,.F.);
#4461=ORIENTED_EDGE('',*,*,#3405,.F.);
#4462=ORIENTED_EDGE('',*,*,#3404,.T.);
#4463=ORIENTED_EDGE('',*,*,#3395,.F.);
#4464=ORIENTED_EDGE('',*,*,#3406,.F.);
#4465=ORIENTED_EDGE('',*,*,#3407,.F.);
#4466=ORIENTED_EDGE('',*,*,#3406,.T.);
#4467=ORIENTED_EDGE('',*,*,#3394,.F.);
#4468=ORIENTED_EDGE('',*,*,#3399,.F.);
#4469=ORIENTED_EDGE('',*,*,#3378,.T.);
#4470=ORIENTED_EDGE('',*,*,#3401,.T.);
#4471=ORIENTED_EDGE('',*,*,#3403,.T.);
#4472=ORIENTED_EDGE('',*,*,#3405,.T.);
#4473=ORIENTED_EDGE('',*,*,#3407,.T.);
#4474=ORIENTED_EDGE('',*,*,#3398,.T.);
#4475=ORIENTED_EDGE('',*,*,#3389,.T.);
#4476=ORIENTED_EDGE('',*,*,#3382,.T.);
#4477=ORIENTED_EDGE('',*,*,#3402,.T.);
#4478=ORIENTED_EDGE('',*,*,#3386,.T.);
#4479=ORIENTED_EDGE('',*,*,#3366,.T.);
#4480=ORIENTED_EDGE('',*,*,#3369,.T.);
#4481=ORIENTED_EDGE('',*,*,#3372,.T.);
#4482=ORIENTED_EDGE('',*,*,#3375,.T.);
#4483=ORIENTED_EDGE('',*,*,#3408,.F.);
#4484=ORIENTED_EDGE('',*,*,#3409,.T.);
#4485=ORIENTED_EDGE('',*,*,#3410,.F.);
#4486=ORIENTED_EDGE('',*,*,#3411,.T.);
#4487=ORIENTED_EDGE('',*,*,#3408,.T.);
#4488=ORIENTED_EDGE('',*,*,#3411,.F.);
#4489=ORIENTED_EDGE('',*,*,#3410,.T.);
#4490=ORIENTED_EDGE('',*,*,#3412,.T.);
#4491=ORIENTED_EDGE('',*,*,#3412,.F.);
#4492=ORIENTED_EDGE('',*,*,#3413,.T.);
#4493=ORIENTED_EDGE('',*,*,#3414,.T.);
#4494=ORIENTED_EDGE('',*,*,#3413,.F.);
#4495=ORIENTED_EDGE('',*,*,#3409,.F.);
#4496=ORIENTED_EDGE('',*,*,#3415,.T.);
#4497=ORIENTED_EDGE('',*,*,#3416,.T.);
#4498=ORIENTED_EDGE('',*,*,#3415,.F.);
#4499=ORIENTED_EDGE('',*,*,#3416,.F.);
#4500=ORIENTED_EDGE('',*,*,#3414,.F.);
#4501=ORIENTED_EDGE('',*,*,#3417,.F.);
#4502=ORIENTED_EDGE('',*,*,#3418,.T.);
#4503=ORIENTED_EDGE('',*,*,#3417,.T.);
#4504=ORIENTED_EDGE('',*,*,#3418,.F.);
#4505=ORIENTED_EDGE('',*,*,#3419,.F.);
#4506=ORIENTED_EDGE('',*,*,#3420,.T.);
#4507=ORIENTED_EDGE('',*,*,#3421,.T.);
#4508=ORIENTED_EDGE('',*,*,#3420,.F.);
#4509=ORIENTED_EDGE('',*,*,#3421,.F.);
#4510=ORIENTED_EDGE('',*,*,#3422,.F.);
#4511=ORIENTED_EDGE('',*,*,#3423,.F.);
#4512=ORIENTED_EDGE('',*,*,#3424,.T.);
#4513=ORIENTED_EDGE('',*,*,#3422,.T.);
#4514=ORIENTED_EDGE('',*,*,#3424,.F.);
#4515=ORIENTED_EDGE('',*,*,#3425,.F.);
#4516=ORIENTED_EDGE('',*,*,#3426,.T.);
#4517=ORIENTED_EDGE('',*,*,#3427,.T.);
#4518=ORIENTED_EDGE('',*,*,#3426,.F.);
#4519=ORIENTED_EDGE('',*,*,#3425,.T.);
#4520=ORIENTED_EDGE('',*,*,#3423,.T.);
#4521=ORIENTED_EDGE('',*,*,#3427,.F.);
#4522=ORIENTED_EDGE('',*,*,#3419,.T.);
#4523=ORIENTED_EDGE('',*,*,#3428,.F.);
#4524=ORIENTED_EDGE('',*,*,#3429,.T.);
#4525=ORIENTED_EDGE('',*,*,#3430,.F.);
#4526=ORIENTED_EDGE('',*,*,#3429,.F.);
#4527=ORIENTED_EDGE('',*,*,#3428,.T.);
#4528=ORIENTED_EDGE('',*,*,#3431,.F.);
#4529=ORIENTED_EDGE('',*,*,#3432,.T.);
#4530=ORIENTED_EDGE('',*,*,#3433,.F.);
#4531=ORIENTED_EDGE('',*,*,#3432,.F.);
#4532=ORIENTED_EDGE('',*,*,#3431,.T.);
#4533=ORIENTED_EDGE('',*,*,#3434,.F.);
#4534=ORIENTED_EDGE('',*,*,#3435,.T.);
#4535=ORIENTED_EDGE('',*,*,#3436,.F.);
#4536=ORIENTED_EDGE('',*,*,#3435,.F.);
#4537=ORIENTED_EDGE('',*,*,#3437,.F.);
#4538=ORIENTED_EDGE('',*,*,#3438,.T.);
#4539=ORIENTED_EDGE('',*,*,#3439,.F.);
#4540=ORIENTED_EDGE('',*,*,#3438,.F.);
#4541=ORIENTED_EDGE('',*,*,#3440,.F.);
#4542=ORIENTED_EDGE('',*,*,#3441,.T.);
#4543=ORIENTED_EDGE('',*,*,#3442,.F.);
#4544=ORIENTED_EDGE('',*,*,#3441,.F.);
#4545=ORIENTED_EDGE('',*,*,#3443,.F.);
#4546=ORIENTED_EDGE('',*,*,#3444,.T.);
#4547=ORIENTED_EDGE('',*,*,#3445,.F.);
#4548=ORIENTED_EDGE('',*,*,#3444,.F.);
#4549=ORIENTED_EDGE('',*,*,#3446,.F.);
#4550=ORIENTED_EDGE('',*,*,#3447,.T.);
#4551=ORIENTED_EDGE('',*,*,#3448,.F.);
#4552=ORIENTED_EDGE('',*,*,#3447,.F.);
#4553=ORIENTED_EDGE('',*,*,#3449,.T.);
#4554=ORIENTED_EDGE('',*,*,#3450,.T.);
#4555=ORIENTED_EDGE('',*,*,#3451,.F.);
#4556=ORIENTED_EDGE('',*,*,#3452,.F.);
#4557=ORIENTED_EDGE('',*,*,#3453,.T.);
#4558=ORIENTED_EDGE('',*,*,#3452,.T.);
#4559=ORIENTED_EDGE('',*,*,#3454,.F.);
#4560=ORIENTED_EDGE('',*,*,#3455,.F.);
#4561=ORIENTED_EDGE('',*,*,#3456,.T.);
#4562=ORIENTED_EDGE('',*,*,#3455,.T.);
#4563=ORIENTED_EDGE('',*,*,#3457,.F.);
#4564=ORIENTED_EDGE('',*,*,#3458,.F.);
#4565=ORIENTED_EDGE('',*,*,#3459,.T.);
#4566=ORIENTED_EDGE('',*,*,#3458,.T.);
#4567=ORIENTED_EDGE('',*,*,#3460,.F.);
#4568=ORIENTED_EDGE('',*,*,#3450,.F.);
#4569=ORIENTED_EDGE('',*,*,#3460,.T.);
#4570=ORIENTED_EDGE('',*,*,#3457,.T.);
#4571=ORIENTED_EDGE('',*,*,#3454,.T.);
#4572=ORIENTED_EDGE('',*,*,#3451,.T.);
#4573=ORIENTED_EDGE('',*,*,#3430,.T.);
#4574=ORIENTED_EDGE('',*,*,#3433,.T.);
#4575=ORIENTED_EDGE('',*,*,#3448,.T.);
#4576=ORIENTED_EDGE('',*,*,#3445,.T.);
#4577=ORIENTED_EDGE('',*,*,#3442,.T.);
#4578=ORIENTED_EDGE('',*,*,#3439,.T.);
#4579=ORIENTED_EDGE('',*,*,#3436,.T.);
#4580=ORIENTED_EDGE('',*,*,#3459,.F.);
#4581=ORIENTED_EDGE('',*,*,#3449,.F.);
#4582=ORIENTED_EDGE('',*,*,#3453,.F.);
#4583=ORIENTED_EDGE('',*,*,#3456,.F.);
#4584=ORIENTED_EDGE('',*,*,#3446,.T.);
#4585=ORIENTED_EDGE('',*,*,#3443,.T.);
#4586=ORIENTED_EDGE('',*,*,#3440,.T.);
#4587=ORIENTED_EDGE('',*,*,#3437,.T.);
#4588=ORIENTED_EDGE('',*,*,#3434,.T.);
#4589=ORIENTED_EDGE('',*,*,#3461,.F.);
#4590=ORIENTED_EDGE('',*,*,#3462,.F.);
#4591=ORIENTED_EDGE('',*,*,#3462,.T.);
#4592=ORIENTED_EDGE('',*,*,#3463,.T.);
#4593=ORIENTED_EDGE('',*,*,#3464,.T.);
#4594=ORIENTED_EDGE('',*,*,#3463,.F.);
#4595=ORIENTED_EDGE('',*,*,#3465,.F.);
#4596=ORIENTED_EDGE('',*,*,#3466,.T.);
#4597=ORIENTED_EDGE('',*,*,#3467,.T.);
#4598=ORIENTED_EDGE('',*,*,#3466,.F.);
#4599=ORIENTED_EDGE('',*,*,#3465,.T.);
#4600=ORIENTED_EDGE('',*,*,#3461,.T.);
#4601=ORIENTED_EDGE('',*,*,#3467,.F.);
#4602=ORIENTED_EDGE('',*,*,#3464,.F.);
#4603=ORIENTED_EDGE('',*,*,#3468,.T.);
#4604=ORIENTED_EDGE('',*,*,#3469,.T.);
#4605=ORIENTED_EDGE('',*,*,#3470,.T.);
#4606=ORIENTED_EDGE('',*,*,#3471,.F.);
#4607=ORIENTED_EDGE('',*,*,#3472,.T.);
#4608=ORIENTED_EDGE('',*,*,#3473,.T.);
#4609=ORIENTED_EDGE('',*,*,#3474,.T.);
#4610=ORIENTED_EDGE('',*,*,#3469,.F.);
#4611=ORIENTED_EDGE('',*,*,#3475,.T.);
#4612=ORIENTED_EDGE('',*,*,#3476,.T.);
#4613=ORIENTED_EDGE('',*,*,#3477,.T.);
#4614=ORIENTED_EDGE('',*,*,#3473,.F.);
#4615=ORIENTED_EDGE('',*,*,#3478,.T.);
#4616=ORIENTED_EDGE('',*,*,#3479,.T.);
#4617=ORIENTED_EDGE('',*,*,#3480,.T.);
#4618=ORIENTED_EDGE('',*,*,#3476,.F.);
#4619=ORIENTED_EDGE('',*,*,#3481,.T.);
#4620=ORIENTED_EDGE('',*,*,#3482,.T.);
#4621=ORIENTED_EDGE('',*,*,#3483,.T.);
#4622=ORIENTED_EDGE('',*,*,#3479,.F.);
#4623=ORIENTED_EDGE('',*,*,#3484,.T.);
#4624=ORIENTED_EDGE('',*,*,#3471,.T.);
#4625=ORIENTED_EDGE('',*,*,#3485,.T.);
#4626=ORIENTED_EDGE('',*,*,#3482,.F.);
#4627=ORIENTED_EDGE('',*,*,#3484,.F.);
#4628=ORIENTED_EDGE('',*,*,#3481,.F.);
#4629=ORIENTED_EDGE('',*,*,#3478,.F.);
#4630=ORIENTED_EDGE('',*,*,#3475,.F.);
#4631=ORIENTED_EDGE('',*,*,#3472,.F.);
#4632=ORIENTED_EDGE('',*,*,#3468,.F.);
#4633=ORIENTED_EDGE('',*,*,#3485,.F.);
#4634=ORIENTED_EDGE('',*,*,#3470,.F.);
#4635=ORIENTED_EDGE('',*,*,#3474,.F.);
#4636=ORIENTED_EDGE('',*,*,#3477,.F.);
#4637=ORIENTED_EDGE('',*,*,#3480,.F.);
#4638=ORIENTED_EDGE('',*,*,#3483,.F.);
#4639=ORIENTED_EDGE('',*,*,#3486,.T.);
#4640=ORIENTED_EDGE('',*,*,#3487,.F.);
#4641=ORIENTED_EDGE('',*,*,#3486,.F.);
#4642=ORIENTED_EDGE('',*,*,#3488,.T.);
#4643=ORIENTED_EDGE('',*,*,#3489,.T.);
#4644=ORIENTED_EDGE('',*,*,#3488,.F.);
#4645=ORIENTED_EDGE('',*,*,#3489,.F.);
#4646=ORIENTED_EDGE('',*,*,#3490,.F.);
#4647=ORIENTED_EDGE('',*,*,#3491,.F.);
#4648=ORIENTED_EDGE('',*,*,#3492,.T.);
#4649=ORIENTED_EDGE('',*,*,#3490,.T.);
#4650=ORIENTED_EDGE('',*,*,#3492,.F.);
#4651=ORIENTED_EDGE('',*,*,#3493,.F.);
#4652=ORIENTED_EDGE('',*,*,#3494,.T.);
#4653=ORIENTED_EDGE('',*,*,#3491,.T.);
#4654=ORIENTED_EDGE('',*,*,#3494,.F.);
#4655=ORIENTED_EDGE('',*,*,#3495,.F.);
#4656=ORIENTED_EDGE('',*,*,#3496,.T.);
#4657=ORIENTED_EDGE('',*,*,#3493,.T.);
#4658=ORIENTED_EDGE('',*,*,#3496,.F.);
#4659=ORIENTED_EDGE('',*,*,#3495,.T.);
#4660=ORIENTED_EDGE('',*,*,#3497,.F.);
#4661=ORIENTED_EDGE('',*,*,#3498,.F.);
#4662=ORIENTED_EDGE('',*,*,#3499,.T.);
#4663=ORIENTED_EDGE('',*,*,#3497,.T.);
#4664=ORIENTED_EDGE('',*,*,#3499,.F.);
#4665=ORIENTED_EDGE('',*,*,#3487,.T.);
#4666=ORIENTED_EDGE('',*,*,#3500,.T.);
#4667=ORIENTED_EDGE('',*,*,#3498,.T.);
#4668=ORIENTED_EDGE('',*,*,#3500,.F.);
#4669=ORIENTED_EDGE('',*,*,#3501,.T.);
#4670=ORIENTED_EDGE('',*,*,#3502,.T.);
#4671=ORIENTED_EDGE('',*,*,#3503,.T.);
#4672=ORIENTED_EDGE('',*,*,#3502,.F.);
#4673=ORIENTED_EDGE('',*,*,#3503,.F.);
#4674=ORIENTED_EDGE('',*,*,#3504,.T.);
#4675=ORIENTED_EDGE('',*,*,#3505,.T.);
#4676=ORIENTED_EDGE('',*,*,#3504,.F.);
#4677=ORIENTED_EDGE('',*,*,#3506,.T.);
#4678=ORIENTED_EDGE('',*,*,#3501,.F.);
#4679=ORIENTED_EDGE('',*,*,#3506,.F.);
#4680=ORIENTED_EDGE('',*,*,#3507,.T.);
#4681=ORIENTED_EDGE('',*,*,#3508,.T.);
#4682=ORIENTED_EDGE('',*,*,#3507,.F.);
#4683=ORIENTED_EDGE('',*,*,#3508,.F.);
#4684=ORIENTED_EDGE('',*,*,#3505,.F.);
#4685=ORIENTED_EDGE('',*,*,#3509,.F.);
#4686=ORIENTED_EDGE('',*,*,#3510,.F.);
#4687=ORIENTED_EDGE('',*,*,#3511,.T.);
#4688=ORIENTED_EDGE('',*,*,#3512,.F.);
#4689=ORIENTED_EDGE('',*,*,#3511,.F.);
#4690=ORIENTED_EDGE('',*,*,#3513,.F.);
#4691=ORIENTED_EDGE('',*,*,#3514,.F.);
#4692=ORIENTED_EDGE('',*,*,#3515,.F.);
#4693=ORIENTED_EDGE('',*,*,#3516,.F.);
#4694=ORIENTED_EDGE('',*,*,#3517,.F.);
#4695=ORIENTED_EDGE('',*,*,#3518,.T.);
#4696=ORIENTED_EDGE('',*,*,#3519,.F.);
#4697=ORIENTED_EDGE('',*,*,#3520,.F.);
#4698=ORIENTED_EDGE('',*,*,#3521,.F.);
#4699=ORIENTED_EDGE('',*,*,#3522,.F.);
#4700=ORIENTED_EDGE('',*,*,#3523,.F.);
#4701=ORIENTED_EDGE('',*,*,#3524,.F.);
#4702=ORIENTED_EDGE('',*,*,#3518,.F.);
#4703=ORIENTED_EDGE('',*,*,#3514,.T.);
#4704=ORIENTED_EDGE('',*,*,#3525,.T.);
#4705=ORIENTED_EDGE('',*,*,#3523,.T.);
#4706=ORIENTED_EDGE('',*,*,#3526,.F.);
#4707=ORIENTED_EDGE('',*,*,#3513,.T.);
#4708=ORIENTED_EDGE('',*,*,#3527,.T.);
#4709=ORIENTED_EDGE('',*,*,#3524,.T.);
#4710=ORIENTED_EDGE('',*,*,#3525,.F.);
#4711=ORIENTED_EDGE('',*,*,#3510,.T.);
#4712=ORIENTED_EDGE('',*,*,#3528,.T.);
#4713=ORIENTED_EDGE('',*,*,#3519,.T.);
#4714=ORIENTED_EDGE('',*,*,#3527,.F.);
#4715=ORIENTED_EDGE('',*,*,#3529,.F.);
#4716=ORIENTED_EDGE('',*,*,#3530,.T.);
#4717=ORIENTED_EDGE('',*,*,#3531,.T.);
#4718=ORIENTED_EDGE('',*,*,#3530,.F.);
#4719=ORIENTED_EDGE('',*,*,#3509,.T.);
#4720=ORIENTED_EDGE('',*,*,#3532,.T.);
#4721=ORIENTED_EDGE('',*,*,#3520,.T.);
#4722=ORIENTED_EDGE('',*,*,#3528,.F.);
#4723=ORIENTED_EDGE('',*,*,#3515,.T.);
#4724=ORIENTED_EDGE('',*,*,#3526,.T.);
#4725=ORIENTED_EDGE('',*,*,#3522,.T.);
#4726=ORIENTED_EDGE('',*,*,#3533,.F.);
#4727=ORIENTED_EDGE('',*,*,#3516,.T.);
#4728=ORIENTED_EDGE('',*,*,#3533,.T.);
#4729=ORIENTED_EDGE('',*,*,#3521,.T.);
#4730=ORIENTED_EDGE('',*,*,#3532,.F.);
#4731=ORIENTED_EDGE('',*,*,#3517,.T.);
#4732=ORIENTED_EDGE('',*,*,#3529,.T.);
#4733=ORIENTED_EDGE('',*,*,#3512,.T.);
#4734=ORIENTED_EDGE('',*,*,#3531,.F.);
#4735=ORIENTED_EDGE('',*,*,#3534,.T.);
#4736=ORIENTED_EDGE('',*,*,#3535,.T.);
#4737=ORIENTED_EDGE('',*,*,#3536,.T.);
#4738=ORIENTED_EDGE('',*,*,#3537,.T.);
#4739=ORIENTED_EDGE('',*,*,#3538,.T.);
#4740=ORIENTED_EDGE('',*,*,#3539,.T.);
#4741=ORIENTED_EDGE('',*,*,#3540,.F.);
#4742=ORIENTED_EDGE('',*,*,#3541,.T.);
#4743=ORIENTED_EDGE('',*,*,#3542,.T.);
#4744=ORIENTED_EDGE('',*,*,#3543,.T.);
#4745=ORIENTED_EDGE('',*,*,#3544,.T.);
#4746=ORIENTED_EDGE('',*,*,#3545,.T.);
#4747=ORIENTED_EDGE('',*,*,#3546,.T.);
#4748=ORIENTED_EDGE('',*,*,#3547,.F.);
#4749=ORIENTED_EDGE('',*,*,#3548,.F.);
#4750=ORIENTED_EDGE('',*,*,#3546,.F.);
#4751=ORIENTED_EDGE('',*,*,#3549,.F.);
#4752=ORIENTED_EDGE('',*,*,#3535,.F.);
#4753=ORIENTED_EDGE('',*,*,#3549,.T.);
#4754=ORIENTED_EDGE('',*,*,#3545,.F.);
#4755=ORIENTED_EDGE('',*,*,#3550,.F.);
#4756=ORIENTED_EDGE('',*,*,#3536,.F.);
#4757=ORIENTED_EDGE('',*,*,#3550,.T.);
#4758=ORIENTED_EDGE('',*,*,#3544,.F.);
#4759=ORIENTED_EDGE('',*,*,#3551,.F.);
#4760=ORIENTED_EDGE('',*,*,#3537,.F.);
#4761=ORIENTED_EDGE('',*,*,#3551,.T.);
#4762=ORIENTED_EDGE('',*,*,#3543,.F.);
#4763=ORIENTED_EDGE('',*,*,#3552,.F.);
#4764=ORIENTED_EDGE('',*,*,#3538,.F.);
#4765=ORIENTED_EDGE('',*,*,#3552,.T.);
#4766=ORIENTED_EDGE('',*,*,#3542,.F.);
#4767=ORIENTED_EDGE('',*,*,#3553,.F.);
#4768=ORIENTED_EDGE('',*,*,#3539,.F.);
#4769=ORIENTED_EDGE('',*,*,#3553,.T.);
#4770=ORIENTED_EDGE('',*,*,#3541,.F.);
#4771=ORIENTED_EDGE('',*,*,#3548,.T.);
#4772=ORIENTED_EDGE('',*,*,#3534,.F.);
#4773=ORIENTED_EDGE('',*,*,#3547,.T.);
#4774=ORIENTED_EDGE('',*,*,#3554,.T.);
#4775=ORIENTED_EDGE('',*,*,#3555,.T.);
#4776=ORIENTED_EDGE('',*,*,#3554,.F.);
#4777=ORIENTED_EDGE('',*,*,#3556,.F.);
#4778=ORIENTED_EDGE('',*,*,#3557,.T.);
#4779=ORIENTED_EDGE('',*,*,#3555,.F.);
#4780=ORIENTED_EDGE('',*,*,#3558,.T.);
#4781=ORIENTED_EDGE('',*,*,#3556,.T.);
#4782=ORIENTED_EDGE('',*,*,#3558,.F.);
#4783=ORIENTED_EDGE('',*,*,#3559,.F.);
#4784=ORIENTED_EDGE('',*,*,#3560,.T.);
#4785=ORIENTED_EDGE('',*,*,#3540,.T.);
#4786=ORIENTED_EDGE('',*,*,#3560,.F.);
#4787=ORIENTED_EDGE('',*,*,#3561,.F.);
#4788=ORIENTED_EDGE('',*,*,#3562,.T.);
#4789=ORIENTED_EDGE('',*,*,#3559,.T.);
#4790=ORIENTED_EDGE('',*,*,#3562,.F.);
#4791=ORIENTED_EDGE('',*,*,#3561,.T.);
#4792=ORIENTED_EDGE('',*,*,#3563,.F.);
#4793=ORIENTED_EDGE('',*,*,#3563,.T.);
#4794=ORIENTED_EDGE('',*,*,#3564,.T.);
#4795=ORIENTED_EDGE('',*,*,#3557,.F.);
#4796=ORIENTED_EDGE('',*,*,#3564,.F.);
#4797=ORIENTED_EDGE('',*,*,#3565,.F.);
#4798=ORIENTED_EDGE('',*,*,#3566,.T.);
#4799=ORIENTED_EDGE('',*,*,#3567,.T.);
#4800=ORIENTED_EDGE('',*,*,#3566,.F.);
#4801=ORIENTED_EDGE('',*,*,#3568,.F.);
#4802=ORIENTED_EDGE('',*,*,#3569,.T.);
#4803=ORIENTED_EDGE('',*,*,#3570,.T.);
#4804=ORIENTED_EDGE('',*,*,#3569,.F.);
#4805=ORIENTED_EDGE('',*,*,#3568,.T.);
#4806=ORIENTED_EDGE('',*,*,#3565,.T.);
#4807=ORIENTED_EDGE('',*,*,#3570,.F.);
#4808=ORIENTED_EDGE('',*,*,#3567,.F.);
#4809=ORIENTED_EDGE('',*,*,#3571,.F.);
#4810=ORIENTED_EDGE('',*,*,#3572,.F.);
#4811=ORIENTED_EDGE('',*,*,#3573,.T.);
#4812=ORIENTED_EDGE('',*,*,#3571,.T.);
#4813=ORIENTED_EDGE('',*,*,#3573,.F.);
#4814=ORIENTED_EDGE('',*,*,#3574,.F.);
#4815=ORIENTED_EDGE('',*,*,#3575,.T.);
#4816=ORIENTED_EDGE('',*,*,#3572,.T.);
#4817=ORIENTED_EDGE('',*,*,#3575,.F.);
#4818=ORIENTED_EDGE('',*,*,#3576,.F.);
#4819=ORIENTED_EDGE('',*,*,#3577,.T.);
#4820=ORIENTED_EDGE('',*,*,#3574,.T.);
#4821=ORIENTED_EDGE('',*,*,#3577,.F.);
#4822=ORIENTED_EDGE('',*,*,#3576,.T.);
#4823=ORIENTED_EDGE('',*,*,#3578,.F.);
#4824=ORIENTED_EDGE('',*,*,#3579,.F.);
#4825=ORIENTED_EDGE('',*,*,#3580,.T.);
#4826=ORIENTED_EDGE('',*,*,#3578,.T.);
#4827=ORIENTED_EDGE('',*,*,#3580,.F.);
#4828=ORIENTED_EDGE('',*,*,#3581,.F.);
#4829=ORIENTED_EDGE('',*,*,#3582,.T.);
#4830=ORIENTED_EDGE('',*,*,#3579,.T.);
#4831=ORIENTED_EDGE('',*,*,#3582,.F.);
#4832=ORIENTED_EDGE('',*,*,#3583,.F.);
#4833=ORIENTED_EDGE('',*,*,#3584,.T.);
#4834=ORIENTED_EDGE('',*,*,#3581,.T.);
#4835=ORIENTED_EDGE('',*,*,#3584,.F.);
#4836=ORIENTED_EDGE('',*,*,#3583,.T.);
#4837=ORIENTED_EDGE('',*,*,#3585,.T.);
#4838=ORIENTED_EDGE('',*,*,#3586,.T.);
#4839=ORIENTED_EDGE('',*,*,#3587,.T.);
#4840=ORIENTED_EDGE('',*,*,#3588,.F.);
#4841=ORIENTED_EDGE('',*,*,#3589,.T.);
#4842=ORIENTED_EDGE('',*,*,#3590,.T.);
#4843=ORIENTED_EDGE('',*,*,#3591,.T.);
#4844=ORIENTED_EDGE('',*,*,#3586,.F.);
#4845=ORIENTED_EDGE('',*,*,#3592,.T.);
#4846=ORIENTED_EDGE('',*,*,#3593,.T.);
#4847=ORIENTED_EDGE('',*,*,#3594,.T.);
#4848=ORIENTED_EDGE('',*,*,#3590,.F.);
#4849=ORIENTED_EDGE('',*,*,#3595,.T.);
#4850=ORIENTED_EDGE('',*,*,#3596,.T.);
#4851=ORIENTED_EDGE('',*,*,#3597,.T.);
#4852=ORIENTED_EDGE('',*,*,#3593,.F.);
#4853=ORIENTED_EDGE('',*,*,#3598,.T.);
#4854=ORIENTED_EDGE('',*,*,#3599,.T.);
#4855=ORIENTED_EDGE('',*,*,#3600,.T.);
#4856=ORIENTED_EDGE('',*,*,#3596,.F.);
#4857=ORIENTED_EDGE('',*,*,#3601,.T.);
#4858=ORIENTED_EDGE('',*,*,#3588,.T.);
#4859=ORIENTED_EDGE('',*,*,#3602,.T.);
#4860=ORIENTED_EDGE('',*,*,#3599,.F.);
#4861=ORIENTED_EDGE('',*,*,#3601,.F.);
#4862=ORIENTED_EDGE('',*,*,#3598,.F.);
#4863=ORIENTED_EDGE('',*,*,#3595,.F.);
#4864=ORIENTED_EDGE('',*,*,#3592,.F.);
#4865=ORIENTED_EDGE('',*,*,#3589,.F.);
#4866=ORIENTED_EDGE('',*,*,#3585,.F.);
#4867=ORIENTED_EDGE('',*,*,#3602,.F.);
#4868=ORIENTED_EDGE('',*,*,#3587,.F.);
#4869=ORIENTED_EDGE('',*,*,#3591,.F.);
#4870=ORIENTED_EDGE('',*,*,#3594,.F.);
#4871=ORIENTED_EDGE('',*,*,#3597,.F.);
#4872=ORIENTED_EDGE('',*,*,#3600,.F.);
#4873=ORIENTED_EDGE('',*,*,#3603,.F.);
#4874=ORIENTED_EDGE('',*,*,#3604,.T.);
#4875=ORIENTED_EDGE('',*,*,#3605,.T.);
#4876=ORIENTED_EDGE('',*,*,#3604,.F.);
#4877=ORIENTED_EDGE('',*,*,#3603,.T.);
#4878=ORIENTED_EDGE('',*,*,#3605,.F.);
#4879=ORIENTED_EDGE('',*,*,#3606,.F.);
#4880=ORIENTED_EDGE('',*,*,#3607,.F.);
#4881=ORIENTED_EDGE('',*,*,#3608,.F.);
#4882=ORIENTED_EDGE('',*,*,#3609,.T.);
#4883=ORIENTED_EDGE('',*,*,#3610,.F.);
#4884=ORIENTED_EDGE('',*,*,#3609,.F.);
#4885=ORIENTED_EDGE('',*,*,#3611,.F.);
#4886=ORIENTED_EDGE('',*,*,#3612,.T.);
#4887=ORIENTED_EDGE('',*,*,#3613,.F.);
#4888=ORIENTED_EDGE('',*,*,#3614,.F.);
#4889=ORIENTED_EDGE('',*,*,#3612,.F.);
#4890=ORIENTED_EDGE('',*,*,#3615,.F.);
#4891=ORIENTED_EDGE('',*,*,#3616,.T.);
#4892=ORIENTED_EDGE('',*,*,#3617,.F.);
#4893=ORIENTED_EDGE('',*,*,#3616,.F.);
#4894=ORIENTED_EDGE('',*,*,#3618,.F.);
#4895=ORIENTED_EDGE('',*,*,#3607,.T.);
#4896=ORIENTED_EDGE('',*,*,#3611,.T.);
#4897=ORIENTED_EDGE('',*,*,#3608,.T.);
#4898=ORIENTED_EDGE('',*,*,#3618,.T.);
#4899=ORIENTED_EDGE('',*,*,#3615,.T.);
#4900=ORIENTED_EDGE('',*,*,#3619,.F.);
#4901=ORIENTED_EDGE('',*,*,#3620,.T.);
#4902=ORIENTED_EDGE('',*,*,#3621,.F.);
#4903=ORIENTED_EDGE('',*,*,#3620,.F.);
#4904=ORIENTED_EDGE('',*,*,#3614,.T.);
#4905=ORIENTED_EDGE('',*,*,#3617,.T.);
#4906=ORIENTED_EDGE('',*,*,#3606,.T.);
#4907=ORIENTED_EDGE('',*,*,#3610,.T.);
#4908=ORIENTED_EDGE('',*,*,#3622,.T.);
#4909=ORIENTED_EDGE('',*,*,#3622,.F.);
#4910=ORIENTED_EDGE('',*,*,#3613,.T.);
#4911=ORIENTED_EDGE('',*,*,#3621,.T.);
#4912=ORIENTED_EDGE('',*,*,#3619,.T.);
#4913=ORIENTED_EDGE('',*,*,#3623,.F.);
#4914=ORIENTED_EDGE('',*,*,#3624,.T.);
#4915=ORIENTED_EDGE('',*,*,#3625,.F.);
#4916=ORIENTED_EDGE('',*,*,#3624,.F.);
#4917=ORIENTED_EDGE('',*,*,#3623,.T.);
#4918=ORIENTED_EDGE('',*,*,#3626,.T.);
#4919=ORIENTED_EDGE('',*,*,#3627,.F.);
#4920=ORIENTED_EDGE('',*,*,#3628,.F.);
#4921=ORIENTED_EDGE('',*,*,#3629,.T.);
#4922=ORIENTED_EDGE('',*,*,#3630,.F.);
#4923=ORIENTED_EDGE('',*,*,#3631,.F.);
#4924=ORIENTED_EDGE('',*,*,#3632,.T.);
#4925=ORIENTED_EDGE('',*,*,#3633,.F.);
#4926=ORIENTED_EDGE('',*,*,#3634,.F.);
#4927=ORIENTED_EDGE('',*,*,#3635,.T.);
#4928=ORIENTED_EDGE('',*,*,#3636,.F.);
#4929=ORIENTED_EDGE('',*,*,#3637,.F.);
#4930=ORIENTED_EDGE('',*,*,#3636,.T.);
#4931=ORIENTED_EDGE('',*,*,#3638,.F.);
#4932=ORIENTED_EDGE('',*,*,#3628,.T.);
#4933=ORIENTED_EDGE('',*,*,#3639,.T.);
#4934=ORIENTED_EDGE('',*,*,#3640,.F.);
#4935=ORIENTED_EDGE('',*,*,#3641,.F.);
#4936=ORIENTED_EDGE('',*,*,#3633,.T.);
#4937=ORIENTED_EDGE('',*,*,#3642,.F.);
#4938=ORIENTED_EDGE('',*,*,#3637,.T.);
#4939=ORIENTED_EDGE('',*,*,#3641,.T.);
#4940=ORIENTED_EDGE('',*,*,#3643,.F.);
#4941=ORIENTED_EDGE('',*,*,#3644,.F.);
#4942=ORIENTED_EDGE('',*,*,#3630,.T.);
#4943=ORIENTED_EDGE('',*,*,#3645,.F.);
#4944=ORIENTED_EDGE('',*,*,#3634,.T.);
#4945=ORIENTED_EDGE('',*,*,#3644,.T.);
#4946=ORIENTED_EDGE('',*,*,#3646,.F.);
#4947=ORIENTED_EDGE('',*,*,#3647,.F.);
#4948=ORIENTED_EDGE('',*,*,#3627,.T.);
#4949=ORIENTED_EDGE('',*,*,#3648,.F.);
#4950=ORIENTED_EDGE('',*,*,#3631,.T.);
#4951=ORIENTED_EDGE('',*,*,#3647,.T.);
#4952=ORIENTED_EDGE('',*,*,#3649,.F.);
#4953=ORIENTED_EDGE('',*,*,#3639,.F.);
#4954=ORIENTED_EDGE('',*,*,#3649,.T.);
#4955=ORIENTED_EDGE('',*,*,#3646,.T.);
#4956=ORIENTED_EDGE('',*,*,#3643,.T.);
#4957=ORIENTED_EDGE('',*,*,#3640,.T.);
#4958=ORIENTED_EDGE('',*,*,#3625,.T.);
#4959=ORIENTED_EDGE('',*,*,#3645,.T.);
#4960=ORIENTED_EDGE('',*,*,#3650,.T.);
#4961=ORIENTED_EDGE('',*,*,#3648,.T.);
#4962=ORIENTED_EDGE('',*,*,#3651,.T.);
#4963=ORIENTED_EDGE('',*,*,#3652,.T.);
#4964=ORIENTED_EDGE('',*,*,#3638,.T.);
#4965=ORIENTED_EDGE('',*,*,#3653,.T.);
#4966=ORIENTED_EDGE('',*,*,#3642,.T.);
#4967=ORIENTED_EDGE('',*,*,#3654,.T.);
#4968=ORIENTED_EDGE('',*,*,#3655,.T.);
#4969=ORIENTED_EDGE('',*,*,#3656,.T.);
#4970=ORIENTED_EDGE('',*,*,#3657,.F.);
#4971=ORIENTED_EDGE('',*,*,#3658,.F.);
#4972=ORIENTED_EDGE('',*,*,#3659,.T.);
#4973=ORIENTED_EDGE('',*,*,#3658,.T.);
#4974=ORIENTED_EDGE('',*,*,#3660,.F.);
#4975=ORIENTED_EDGE('',*,*,#3661,.F.);
#4976=ORIENTED_EDGE('',*,*,#3662,.T.);
#4977=ORIENTED_EDGE('',*,*,#3661,.T.);
#4978=ORIENTED_EDGE('',*,*,#3663,.F.);
#4979=ORIENTED_EDGE('',*,*,#3664,.F.);
#4980=ORIENTED_EDGE('',*,*,#3665,.T.);
#4981=ORIENTED_EDGE('',*,*,#3664,.T.);
#4982=ORIENTED_EDGE('',*,*,#3666,.F.);
#4983=ORIENTED_EDGE('',*,*,#3656,.F.);
#4984=ORIENTED_EDGE('',*,*,#3665,.F.);
#4985=ORIENTED_EDGE('',*,*,#3655,.F.);
#4986=ORIENTED_EDGE('',*,*,#3659,.F.);
#4987=ORIENTED_EDGE('',*,*,#3662,.F.);
#4988=ORIENTED_EDGE('',*,*,#3651,.F.);
#4989=ORIENTED_EDGE('',*,*,#3626,.F.);
#4990=ORIENTED_EDGE('',*,*,#3653,.F.);
#4991=ORIENTED_EDGE('',*,*,#3635,.F.);
#4992=ORIENTED_EDGE('',*,*,#3654,.F.);
#4993=ORIENTED_EDGE('',*,*,#3632,.F.);
#4994=ORIENTED_EDGE('',*,*,#3650,.F.);
#4995=ORIENTED_EDGE('',*,*,#3629,.F.);
#4996=ORIENTED_EDGE('',*,*,#3652,.F.);
#4997=ORIENTED_EDGE('',*,*,#3667,.T.);
#4998=ORIENTED_EDGE('',*,*,#3668,.T.);
#4999=ORIENTED_EDGE('',*,*,#3667,.F.);
#5000=ORIENTED_EDGE('',*,*,#3668,.F.);
#5001=ORIENTED_EDGE('',*,*,#3657,.T.);
#5002=ORIENTED_EDGE('',*,*,#3666,.T.);
#5003=ORIENTED_EDGE('',*,*,#3663,.T.);
#5004=ORIENTED_EDGE('',*,*,#3660,.T.);
#5005=ORIENTED_EDGE('',*,*,#3669,.F.);
#5006=ORIENTED_EDGE('',*,*,#3670,.F.);
#5007=ORIENTED_EDGE('',*,*,#3671,.F.);
#5008=ORIENTED_EDGE('',*,*,#3672,.T.);
#5009=ORIENTED_EDGE('',*,*,#3673,.F.);
#5010=ORIENTED_EDGE('',*,*,#3672,.F.);
#5011=ORIENTED_EDGE('',*,*,#3674,.F.);
#5012=ORIENTED_EDGE('',*,*,#3675,.T.);
#5013=ORIENTED_EDGE('',*,*,#3676,.F.);
#5014=ORIENTED_EDGE('',*,*,#3675,.F.);
#5015=ORIENTED_EDGE('',*,*,#3677,.F.);
#5016=ORIENTED_EDGE('',*,*,#3678,.T.);
#5017=ORIENTED_EDGE('',*,*,#3679,.F.);
#5018=ORIENTED_EDGE('',*,*,#3678,.F.);
#5019=ORIENTED_EDGE('',*,*,#3680,.F.);
#5020=ORIENTED_EDGE('',*,*,#3670,.T.);
#5021=ORIENTED_EDGE('',*,*,#3681,.T.);
#5022=ORIENTED_EDGE('',*,*,#3682,.T.);
#5023=ORIENTED_EDGE('',*,*,#3683,.F.);
#5024=ORIENTED_EDGE('',*,*,#3684,.F.);
#5025=ORIENTED_EDGE('',*,*,#3685,.T.);
#5026=ORIENTED_EDGE('',*,*,#3684,.T.);
#5027=ORIENTED_EDGE('',*,*,#3686,.F.);
#5028=ORIENTED_EDGE('',*,*,#3687,.F.);
#5029=ORIENTED_EDGE('',*,*,#3688,.T.);
#5030=ORIENTED_EDGE('',*,*,#3687,.T.);
#5031=ORIENTED_EDGE('',*,*,#3689,.F.);
#5032=ORIENTED_EDGE('',*,*,#3690,.F.);
#5033=ORIENTED_EDGE('',*,*,#3691,.T.);
#5034=ORIENTED_EDGE('',*,*,#3690,.T.);
#5035=ORIENTED_EDGE('',*,*,#3692,.F.);
#5036=ORIENTED_EDGE('',*,*,#3682,.F.);
#5037=ORIENTED_EDGE('',*,*,#3692,.T.);
#5038=ORIENTED_EDGE('',*,*,#3689,.T.);
#5039=ORIENTED_EDGE('',*,*,#3686,.T.);
#5040=ORIENTED_EDGE('',*,*,#3683,.T.);
#5041=ORIENTED_EDGE('',*,*,#3676,.T.);
#5042=ORIENTED_EDGE('',*,*,#3679,.T.);
#5043=ORIENTED_EDGE('',*,*,#3669,.T.);
#5044=ORIENTED_EDGE('',*,*,#3673,.T.);
#5045=ORIENTED_EDGE('',*,*,#3691,.F.);
#5046=ORIENTED_EDGE('',*,*,#3681,.F.);
#5047=ORIENTED_EDGE('',*,*,#3685,.F.);
#5048=ORIENTED_EDGE('',*,*,#3688,.F.);
#5049=ORIENTED_EDGE('',*,*,#3677,.T.);
#5050=ORIENTED_EDGE('',*,*,#3674,.T.);
#5051=ORIENTED_EDGE('',*,*,#3671,.T.);
#5052=ORIENTED_EDGE('',*,*,#3680,.T.);
#5053=ORIENTED_EDGE('',*,*,#3693,.F.);
#5054=ORIENTED_EDGE('',*,*,#3694,.T.);
#5055=ORIENTED_EDGE('',*,*,#3695,.T.);
#5056=ORIENTED_EDGE('',*,*,#3694,.F.);
#5057=ORIENTED_EDGE('',*,*,#3696,.F.);
#5058=ORIENTED_EDGE('',*,*,#3697,.T.);
#5059=ORIENTED_EDGE('',*,*,#3698,.T.);
#5060=ORIENTED_EDGE('',*,*,#3697,.F.);
#5061=ORIENTED_EDGE('',*,*,#3696,.T.);
#5062=ORIENTED_EDGE('',*,*,#3693,.T.);
#5063=ORIENTED_EDGE('',*,*,#3698,.F.);
#5064=ORIENTED_EDGE('',*,*,#3695,.F.);
#5065=ORIENTED_EDGE('',*,*,#3699,.T.);
#5066=ORIENTED_EDGE('',*,*,#3700,.T.);
#5067=ORIENTED_EDGE('',*,*,#3701,.F.);
#5068=ORIENTED_EDGE('',*,*,#3702,.F.);
#5069=ORIENTED_EDGE('',*,*,#3703,.T.);
#5070=ORIENTED_EDGE('',*,*,#3702,.T.);
#5071=ORIENTED_EDGE('',*,*,#3704,.F.);
#5072=ORIENTED_EDGE('',*,*,#3705,.F.);
#5073=ORIENTED_EDGE('',*,*,#3706,.T.);
#5074=ORIENTED_EDGE('',*,*,#3705,.T.);
#5075=ORIENTED_EDGE('',*,*,#3707,.F.);
#5076=ORIENTED_EDGE('',*,*,#3708,.F.);
#5077=ORIENTED_EDGE('',*,*,#3709,.T.);
#5078=ORIENTED_EDGE('',*,*,#3708,.T.);
#5079=ORIENTED_EDGE('',*,*,#3710,.F.);
#5080=ORIENTED_EDGE('',*,*,#3700,.F.);
#5081=ORIENTED_EDGE('',*,*,#3710,.T.);
#5082=ORIENTED_EDGE('',*,*,#3707,.T.);
#5083=ORIENTED_EDGE('',*,*,#3704,.T.);
#5084=ORIENTED_EDGE('',*,*,#3701,.T.);
#5085=ORIENTED_EDGE('',*,*,#3709,.F.);
#5086=ORIENTED_EDGE('',*,*,#3699,.F.);
#5087=ORIENTED_EDGE('',*,*,#3703,.F.);
#5088=ORIENTED_EDGE('',*,*,#3706,.F.);
#5089=ORIENTED_EDGE('',*,*,#3711,.T.);
#5090=ORIENTED_EDGE('',*,*,#3712,.T.);
#5091=ORIENTED_EDGE('',*,*,#3713,.T.);
#5092=ORIENTED_EDGE('',*,*,#3714,.F.);
#5093=ORIENTED_EDGE('',*,*,#3715,.T.);
#5094=ORIENTED_EDGE('',*,*,#3716,.T.);
#5095=ORIENTED_EDGE('',*,*,#3717,.T.);
#5096=ORIENTED_EDGE('',*,*,#3712,.F.);
#5097=ORIENTED_EDGE('',*,*,#3718,.T.);
#5098=ORIENTED_EDGE('',*,*,#3719,.T.);
#5099=ORIENTED_EDGE('',*,*,#3720,.T.);
#5100=ORIENTED_EDGE('',*,*,#3716,.F.);
#5101=ORIENTED_EDGE('',*,*,#3721,.T.);
#5102=ORIENTED_EDGE('',*,*,#3722,.T.);
#5103=ORIENTED_EDGE('',*,*,#3723,.T.);
#5104=ORIENTED_EDGE('',*,*,#3719,.F.);
#5105=ORIENTED_EDGE('',*,*,#3724,.T.);
#5106=ORIENTED_EDGE('',*,*,#3725,.T.);
#5107=ORIENTED_EDGE('',*,*,#3726,.T.);
#5108=ORIENTED_EDGE('',*,*,#3722,.F.);
#5109=ORIENTED_EDGE('',*,*,#3727,.T.);
#5110=ORIENTED_EDGE('',*,*,#3714,.T.);
#5111=ORIENTED_EDGE('',*,*,#3728,.T.);
#5112=ORIENTED_EDGE('',*,*,#3725,.F.);
#5113=ORIENTED_EDGE('',*,*,#3727,.F.);
#5114=ORIENTED_EDGE('',*,*,#3724,.F.);
#5115=ORIENTED_EDGE('',*,*,#3721,.F.);
#5116=ORIENTED_EDGE('',*,*,#3718,.F.);
#5117=ORIENTED_EDGE('',*,*,#3715,.F.);
#5118=ORIENTED_EDGE('',*,*,#3711,.F.);
#5119=ORIENTED_EDGE('',*,*,#3728,.F.);
#5120=ORIENTED_EDGE('',*,*,#3713,.F.);
#5121=ORIENTED_EDGE('',*,*,#3717,.F.);
#5122=ORIENTED_EDGE('',*,*,#3720,.F.);
#5123=ORIENTED_EDGE('',*,*,#3723,.F.);
#5124=ORIENTED_EDGE('',*,*,#3726,.F.);
#5125=ORIENTED_EDGE('',*,*,#3729,.F.);
#5126=ORIENTED_EDGE('',*,*,#3730,.F.);
#5127=ORIENTED_EDGE('',*,*,#3731,.F.);
#5128=ORIENTED_EDGE('',*,*,#3732,.T.);
#5129=ORIENTED_EDGE('',*,*,#3730,.T.);
#5130=ORIENTED_EDGE('',*,*,#3732,.F.);
#5131=ORIENTED_EDGE('',*,*,#3733,.F.);
#5132=ORIENTED_EDGE('',*,*,#3734,.T.);
#5133=ORIENTED_EDGE('',*,*,#3731,.T.);
#5134=ORIENTED_EDGE('',*,*,#3734,.F.);
#5135=ORIENTED_EDGE('',*,*,#3735,.F.);
#5136=ORIENTED_EDGE('',*,*,#3736,.T.);
#5137=ORIENTED_EDGE('',*,*,#3733,.T.);
#5138=ORIENTED_EDGE('',*,*,#3736,.F.);
#5139=ORIENTED_EDGE('',*,*,#3735,.T.);
#5140=ORIENTED_EDGE('',*,*,#3737,.F.);
#5141=ORIENTED_EDGE('',*,*,#3738,.F.);
#5142=ORIENTED_EDGE('',*,*,#3739,.T.);
#5143=ORIENTED_EDGE('',*,*,#3737,.T.);
#5144=ORIENTED_EDGE('',*,*,#3739,.F.);
#5145=ORIENTED_EDGE('',*,*,#3729,.T.);
#5146=ORIENTED_EDGE('',*,*,#3740,.T.);
#5147=ORIENTED_EDGE('',*,*,#3738,.T.);
#5148=ORIENTED_EDGE('',*,*,#3740,.F.);
#5149=CYLINDRICAL_SURFACE('',#5898,0.25);
#5150=CYLINDRICAL_SURFACE('',#5902,0.25);
#5151=CYLINDRICAL_SURFACE('',#5906,0.93);
#5152=CYLINDRICAL_SURFACE('',#5911,0.93);
#5153=CYLINDRICAL_SURFACE('',#5918,0.789999999999999);
#5154=CYLINDRICAL_SURFACE('',#5921,0.789999999999999);
#5155=CYLINDRICAL_SURFACE('',#5925,0.789999999999999);
#5156=CYLINDRICAL_SURFACE('',#5929,0.789999999999999);
#5157=CYLINDRICAL_SURFACE('',#5934,0.79);
#5158=CYLINDRICAL_SURFACE('',#5961,0.93);
#5159=CYLINDRICAL_SURFACE('',#5967,0.789999999999999);
#5160=CYLINDRICAL_SURFACE('',#5968,0.789999999999999);
#5161=CYLINDRICAL_SURFACE('',#5970,0.789999999999999);
#5162=CYLINDRICAL_SURFACE('',#5972,0.789999999999999);
#5163=CYLINDRICAL_SURFACE('',#5977,0.93);
#5164=CYLINDRICAL_SURFACE('',#5983,0.789999999999999);
#5165=CYLINDRICAL_SURFACE('',#5984,0.789999999999999);
#5166=CYLINDRICAL_SURFACE('',#5986,0.789999999999999);
#5167=CYLINDRICAL_SURFACE('',#5988,0.789999999999999);
#5168=CYLINDRICAL_SURFACE('',#5993,0.93);
#5169=CYLINDRICAL_SURFACE('',#5999,0.79);
#5170=CYLINDRICAL_SURFACE('',#6000,0.79);
#5171=CYLINDRICAL_SURFACE('',#6002,0.79);
#5172=CYLINDRICAL_SURFACE('',#6004,0.79);
#5173=CYLINDRICAL_SURFACE('',#6009,0.93);
#5174=CYLINDRICAL_SURFACE('',#6029,0.93);
#5175=CYLINDRICAL_SURFACE('',#6033,0.55);
#5176=CYLINDRICAL_SURFACE('',#6038,0.33);
#5177=CYLINDRICAL_SURFACE('',#6040,0.55);
#5178=CYLINDRICAL_SURFACE('',#6045,0.33);
#5179=CYLINDRICAL_SURFACE('',#6047,0.6);
#5180=CYLINDRICAL_SURFACE('',#6052,0.33);
#5181=CYLINDRICAL_SURFACE('',#6061,0.549999999999997);
#5182=CYLINDRICAL_SURFACE('',#6066,0.329999999999998);
#5183=CYLINDRICAL_SURFACE('',#6068,0.549999999999997);
#5184=CYLINDRICAL_SURFACE('',#6073,0.329999999999998);
#5185=CYLINDRICAL_SURFACE('',#6075,0.600000000000001);
#5186=CYLINDRICAL_SURFACE('',#6080,0.329999999999998);
#5187=CYLINDRICAL_SURFACE('',#6089,0.2942);
#5188=CYLINDRICAL_SURFACE('',#6107,0.165);
#5189=CYLINDRICAL_SURFACE('',#6111,0.165);
#5190=CYLINDRICAL_SURFACE('',#6115,0.275);
#5191=CYLINDRICAL_SURFACE('',#6118,0.275);
#5192=CYLINDRICAL_SURFACE('',#6121,0.275);
#5193=CYLINDRICAL_SURFACE('',#6124,0.275);
#5194=CYLINDRICAL_SURFACE('',#6127,0.7);
#5195=CYLINDRICAL_SURFACE('',#6133,0.93);
#5196=CYLINDRICAL_SURFACE('',#6136,1.3);
#5197=CYLINDRICAL_SURFACE('',#6150,0.165);
#5198=CYLINDRICAL_SURFACE('',#6154,0.165);
#5199=CYLINDRICAL_SURFACE('',#6158,0.275);
#5200=CYLINDRICAL_SURFACE('',#6161,0.275);
#5201=CYLINDRICAL_SURFACE('',#6164,0.275);
#5202=CYLINDRICAL_SURFACE('',#6167,0.275);
#5203=CYLINDRICAL_SURFACE('',#6170,0.7);
#5204=CYLINDRICAL_SURFACE('',#6176,0.93);
#5205=CYLINDRICAL_SURFACE('',#6179,1.3);
#5206=CYLINDRICAL_SURFACE('',#6193,0.275);
#5207=CYLINDRICAL_SURFACE('',#6196,0.275);
#5208=CYLINDRICAL_SURFACE('',#6199,0.275);
#5209=CYLINDRICAL_SURFACE('',#6202,0.275);
#5210=CYLINDRICAL_SURFACE('',#6213,1.6);
#5211=CYLINDRICAL_SURFACE('',#6223,1.2);
#5212=CYLINDRICAL_SURFACE('',#6227,0.405);
#5213=CYLINDRICAL_SURFACE('',#6229,0.7);
#5214=CYLINDRICAL_SURFACE('',#6237,0.61);
#5215=CYLINDRICAL_SURFACE('',#6242,0.405);
#5216=CYLINDRICAL_SURFACE('',#6244,1.);
#5217=CYLINDRICAL_SURFACE('',#6250,0.3);
#5218=CYLINDRICAL_SURFACE('',#6254,0.3);
#5219=CYLINDRICAL_SURFACE('',#6258,0.225);
#5220=CYLINDRICAL_SURFACE('',#6261,0.225);
#5221=CYLINDRICAL_SURFACE('',#6264,0.225);
#5222=CYLINDRICAL_SURFACE('',#6267,0.225);
#5223=CYLINDRICAL_SURFACE('',#6270,1.01);
#5224=CYLINDRICAL_SURFACE('',#6283,0.75);
#5225=CYLINDRICAL_SURFACE('',#6285,1.3);
#5226=CYLINDRICAL_SURFACE('',#6302,0.25);
#5227=CYLINDRICAL_SURFACE('',#6309,0.425);
#5228=CYLINDRICAL_SURFACE('',#6317,0.24505);
#5229=CYLINDRICAL_SURFACE('',#6322,0.265);
#5230=CYLINDRICAL_SURFACE('',#6326,0.5);
#5231=CYLINDRICAL_SURFACE('',#6337,0.2117);
#5232=CYLINDRICAL_SURFACE('',#6356,1.065);
#5233=CYLINDRICAL_SURFACE('',#6362,1.065);
#5234=CYLINDRICAL_SURFACE('',#6368,0.79);
#5235=CYLINDRICAL_SURFACE('',#6370,0.225);
#5236=CYLINDRICAL_SURFACE('',#6373,0.4);
#5237=CYLINDRICAL_SURFACE('',#6383,0.35);
#5238=CYLINDRICAL_SURFACE('',#6391,0.1954);
#5239=CYLINDRICAL_SURFACE('',#6405,0.3);
#5240=CYLINDRICAL_SURFACE('',#6422,0.75);
#5241=CYLINDRICAL_SURFACE('',#6428,0.165);
#5242=CYLINDRICAL_SURFACE('',#6459,0.4);
#5243=CYLINDRICAL_SURFACE('',#6474,0.225);
#5244=CYLINDRICAL_SURFACE('',#6477,0.6);
#5245=CYLINDRICAL_SURFACE('',#6504,0.35);
#5246=CYLINDRICAL_SURFACE('',#6512,0.1954);
#5247=ADVANCED_FACE('',(#747),#5149,.F.);
#5248=ADVANCED_FACE('',(#748),#535,.F.);
#5249=ADVANCED_FACE('',(#749),#5150,.F.);
#5250=ADVANCED_FACE('',(#750),#536,.F.);
#5251=ADVANCED_FACE('',(#751),#5151,.F.);
#5252=ADVANCED_FACE('',(#752,#426),#537,.T.);
#5253=ADVANCED_FACE('',(#753),#5152,.F.);
#5254=ADVANCED_FACE('',(#754,#427),#538,.F.);
#5255=ADVANCED_FACE('',(#755),#539,.F.);
#5256=ADVANCED_FACE('',(#756),#5153,.F.);
#5257=ADVANCED_FACE('',(#757),#5154,.F.);
#5258=ADVANCED_FACE('',(#758),#5155,.F.);
#5259=ADVANCED_FACE('',(#759),#5156,.F.);
#5260=ADVANCED_FACE('',(#760),#540,.F.);
#5261=ADVANCED_FACE('',(#761),#5157,.F.);
#5262=ADVANCED_FACE('',(#762),#541,.F.);
#5263=ADVANCED_FACE('',(#763),#5158,.F.);
#5264=ADVANCED_FACE('',(#764),#542,.F.);
#5265=ADVANCED_FACE('',(#765),#543,.F.);
#5266=ADVANCED_FACE('',(#766),#5159,.F.);
#5267=ADVANCED_FACE('',(#767),#5160,.F.);
#5268=ADVANCED_FACE('',(#768),#5161,.F.);
#5269=ADVANCED_FACE('',(#769),#5162,.F.);
#5270=ADVANCED_FACE('',(#770),#544,.F.);
#5271=ADVANCED_FACE('',(#771),#545,.F.);
#5272=ADVANCED_FACE('',(#772),#5163,.F.);
#5273=ADVANCED_FACE('',(#773),#546,.F.);
#5274=ADVANCED_FACE('',(#774),#547,.F.);
#5275=ADVANCED_FACE('',(#775),#5164,.F.);
#5276=ADVANCED_FACE('',(#776),#5165,.F.);
#5277=ADVANCED_FACE('',(#777),#5166,.F.);
#5278=ADVANCED_FACE('',(#778),#5167,.F.);
#5279=ADVANCED_FACE('',(#779),#548,.F.);
#5280=ADVANCED_FACE('',(#780),#549,.F.);
#5281=ADVANCED_FACE('',(#781),#5168,.F.);
#5282=ADVANCED_FACE('',(#782),#550,.F.);
#5283=ADVANCED_FACE('',(#783),#551,.F.);
#5284=ADVANCED_FACE('',(#784),#5169,.F.);
#5285=ADVANCED_FACE('',(#785),#5170,.F.);
#5286=ADVANCED_FACE('',(#786),#5171,.F.);
#5287=ADVANCED_FACE('',(#787),#5172,.F.);
#5288=ADVANCED_FACE('',(#788),#552,.F.);
#5289=ADVANCED_FACE('',(#789),#553,.F.);
#5290=ADVANCED_FACE('',(#790),#5173,.F.);
#5291=ADVANCED_FACE('',(#791),#554,.F.);
#5292=ADVANCED_FACE('',(#792),#555,.T.);
#5293=ADVANCED_FACE('',(#793,#428),#556,.T.);
#5294=ADVANCED_FACE('',(#794,#429,#430,#431,#432),#557,.T.);
#5295=ADVANCED_FACE('',(#795,#433),#558,.T.);
#5296=ADVANCED_FACE('',(#796),#559,.T.);
#5297=ADVANCED_FACE('',(#797,#434,#435),#560,.F.);
#5298=ADVANCED_FACE('',(#798,#436),#561,.T.);
#5299=ADVANCED_FACE('',(#799),#562,.T.);
#5300=ADVANCED_FACE('',(#800),#563,.T.);
#5301=ADVANCED_FACE('',(#801),#564,.T.);
#5302=ADVANCED_FACE('',(#802),#565,.T.);
#5303=ADVANCED_FACE('',(#803),#566,.T.);
#5304=ADVANCED_FACE('',(#804),#567,.T.);
#5305=ADVANCED_FACE('',(#805),#568,.F.);
#5306=ADVANCED_FACE('',(#806),#5174,.T.);
#5307=ADVANCED_FACE('',(#807),#569,.T.);
#5308=ADVANCED_FACE('',(#808),#5175,.F.);
#5309=ADVANCED_FACE('',(#809,#437),#570,.T.);
#5310=ADVANCED_FACE('',(#810),#5176,.F.);
#5311=ADVANCED_FACE('',(#811),#5177,.F.);
#5312=ADVANCED_FACE('',(#812,#438),#571,.T.);
#5313=ADVANCED_FACE('',(#813),#5178,.F.);
#5314=ADVANCED_FACE('',(#814),#5179,.F.);
#5315=ADVANCED_FACE('',(#815,#439),#572,.F.);
#5316=ADVANCED_FACE('',(#816),#5180,.F.);
#5317=ADVANCED_FACE('',(#817),#573,.T.);
#5318=ADVANCED_FACE('',(#818),#574,.T.);
#5319=ADVANCED_FACE('',(#819),#575,.T.);
#5320=ADVANCED_FACE('',(#820),#576,.T.);
#5321=ADVANCED_FACE('',(#821,#440,#441,#442),#577,.T.);
#5322=ADVANCED_FACE('',(#822,#443,#444,#445),#578,.F.);
#5323=ADVANCED_FACE('',(#823),#5181,.F.);
#5324=ADVANCED_FACE('',(#824,#446),#579,.T.);
#5325=ADVANCED_FACE('',(#825),#5182,.F.);
#5326=ADVANCED_FACE('',(#826),#5183,.F.);
#5327=ADVANCED_FACE('',(#827,#447),#580,.T.);
#5328=ADVANCED_FACE('',(#828),#5184,.F.);
#5329=ADVANCED_FACE('',(#829),#5185,.F.);
#5330=ADVANCED_FACE('',(#830,#448),#581,.F.);
#5331=ADVANCED_FACE('',(#831),#5186,.F.);
#5332=ADVANCED_FACE('',(#832),#582,.T.);
#5333=ADVANCED_FACE('',(#833),#583,.T.);
#5334=ADVANCED_FACE('',(#834),#584,.T.);
#5335=ADVANCED_FACE('',(#835),#585,.T.);
#5336=ADVANCED_FACE('',(#836,#449,#450,#451),#586,.T.);
#5337=ADVANCED_FACE('',(#837,#452,#453,#454),#587,.F.);
#5338=ADVANCED_FACE('',(#838),#5187,.T.);
#5339=ADVANCED_FACE('',(#839),#264,.T.);
#5340=ADVANCED_FACE('',(#840),#588,.T.);
#5341=ADVANCED_FACE('',(#841),#265,.T.);
#5342=ADVANCED_FACE('',(#842),#589,.T.);
#5343=ADVANCED_FACE('',(#843),#590,.T.);
#5344=ADVANCED_FACE('',(#844),#591,.T.);
#5345=ADVANCED_FACE('',(#845),#592,.T.);
#5346=ADVANCED_FACE('',(#846),#593,.T.);
#5347=ADVANCED_FACE('',(#847),#594,.T.);
#5348=ADVANCED_FACE('',(#848),#595,.T.);
#5349=ADVANCED_FACE('',(#849,#455),#596,.F.);
#5350=ADVANCED_FACE('',(#850),#5188,.F.);
#5351=ADVANCED_FACE('',(#851),#597,.T.);
#5352=ADVANCED_FACE('',(#852),#5189,.F.);
#5353=ADVANCED_FACE('',(#853),#598,.T.);
#5354=ADVANCED_FACE('',(#854),#5190,.F.);
#5355=ADVANCED_FACE('',(#855),#5191,.F.);
#5356=ADVANCED_FACE('',(#856),#5192,.F.);
#5357=ADVANCED_FACE('',(#857),#5193,.F.);
#5358=ADVANCED_FACE('',(#858),#5194,.F.);
#5359=ADVANCED_FACE('',(#859),#599,.T.);
#5360=ADVANCED_FACE('',(#860,#456,#457),#600,.T.);
#5361=ADVANCED_FACE('',(#861),#5195,.F.);
#5362=ADVANCED_FACE('',(#862),#5196,.F.);
#5363=ADVANCED_FACE('',(#863,#458),#601,.F.);
#5364=ADVANCED_FACE('',(#864,#459),#602,.T.);
#5365=ADVANCED_FACE('',(#865,#460),#242,.F.);
#5366=ADVANCED_FACE('',(#866,#461,#462,#463,#464),#603,.T.);
#5367=ADVANCED_FACE('',(#867),#604,.T.);
#5368=ADVANCED_FACE('',(#868,#465,#466,#467,#468,#469),#605,.T.);
#5369=ADVANCED_FACE('',(#869),#606,.T.);
#5370=ADVANCED_FACE('',(#870),#607,.F.);
#5371=ADVANCED_FACE('',(#871),#5197,.F.);
#5372=ADVANCED_FACE('',(#872),#608,.T.);
#5373=ADVANCED_FACE('',(#873),#5198,.F.);
#5374=ADVANCED_FACE('',(#874),#609,.T.);
#5375=ADVANCED_FACE('',(#875),#5199,.F.);
#5376=ADVANCED_FACE('',(#876),#5200,.F.);
#5377=ADVANCED_FACE('',(#877),#5201,.F.);
#5378=ADVANCED_FACE('',(#878),#5202,.F.);
#5379=ADVANCED_FACE('',(#879),#5203,.F.);
#5380=ADVANCED_FACE('',(#880),#610,.T.);
#5381=ADVANCED_FACE('',(#881,#470,#471),#611,.T.);
#5382=ADVANCED_FACE('',(#882),#5204,.F.);
#5383=ADVANCED_FACE('',(#883),#5205,.F.);
#5384=ADVANCED_FACE('',(#884,#472),#612,.F.);
#5385=ADVANCED_FACE('',(#885,#473),#613,.T.);
#5386=ADVANCED_FACE('',(#886,#474),#243,.F.);
#5387=ADVANCED_FACE('',(#887,#475,#476,#477,#478,#479),#614,.T.);
#5388=ADVANCED_FACE('',(#888),#615,.T.);
#5389=ADVANCED_FACE('',(#889,#480,#481,#482,#483),#616,.T.);
#5390=ADVANCED_FACE('',(#890),#617,.T.);
#5391=ADVANCED_FACE('',(#891),#618,.F.);
#5392=ADVANCED_FACE('',(#892),#5206,.F.);
#5393=ADVANCED_FACE('',(#893),#5207,.F.);
#5394=ADVANCED_FACE('',(#894),#5208,.F.);
#5395=ADVANCED_FACE('',(#895),#5209,.F.);
#5396=ADVANCED_FACE('',(#896),#619,.F.);
#5397=ADVANCED_FACE('',(#897),#620,.F.);
#5398=ADVANCED_FACE('',(#898),#621,.F.);
#5399=ADVANCED_FACE('',(#899),#622,.F.);
#5400=ADVANCED_FACE('',(#900,#484,#485,#486,#487),#623,.T.);
#5401=ADVANCED_FACE('',(#901),#624,.T.);
#5402=ADVANCED_FACE('',(#902),#625,.T.);
#5403=ADVANCED_FACE('',(#903),#5210,.F.);
#5404=ADVANCED_FACE('',(#904),#626,.T.);
#5405=ADVANCED_FACE('',(#905),#627,.T.);
#5406=ADVANCED_FACE('',(#906),#628,.T.);
#5407=ADVANCED_FACE('',(#907,#488,#489,#490,#491),#629,.F.);
#5408=ADVANCED_FACE('',(#908,#492),#630,.F.);
#5409=ADVANCED_FACE('',(#909),#5211,.T.);
#5410=ADVANCED_FACE('',(#910,#493),#631,.T.);
#5411=ADVANCED_FACE('',(#911),#5212,.F.);
#5412=ADVANCED_FACE('',(#912),#5213,.T.);
#5413=ADVANCED_FACE('',(#913,#494),#632,.F.);
#5414=ADVANCED_FACE('',(#914),#241,.T.);
#5415=ADVANCED_FACE('',(#915),#5214,.F.);
#5416=ADVANCED_FACE('',(#916,#495),#633,.F.);
#5417=ADVANCED_FACE('',(#917),#5215,.F.);
#5418=ADVANCED_FACE('',(#918),#5216,.T.);
#5419=ADVANCED_FACE('',(#919,#496),#634,.T.);
#5420=ADVANCED_FACE('',(#920,#497),#635,.F.);
#5421=ADVANCED_FACE('',(#921),#5217,.F.);
#5422=ADVANCED_FACE('',(#922),#636,.T.);
#5423=ADVANCED_FACE('',(#923),#5218,.F.);
#5424=ADVANCED_FACE('',(#924),#637,.T.);
#5425=ADVANCED_FACE('',(#925),#5219,.F.);
#5426=ADVANCED_FACE('',(#926),#5220,.F.);
#5427=ADVANCED_FACE('',(#927),#5221,.F.);
#5428=ADVANCED_FACE('',(#928),#5222,.F.);
#5429=ADVANCED_FACE('',(#929),#5223,.F.);
#5430=ADVANCED_FACE('',(#930),#638,.T.);
#5431=ADVANCED_FACE('',(#931),#639,.T.);
#5432=ADVANCED_FACE('',(#932),#640,.T.);
#5433=ADVANCED_FACE('',(#933),#641,.T.);
#5434=ADVANCED_FACE('',(#934,#498,#499,#500,#501,#502,#503,#504),#642,.T.);
#5435=ADVANCED_FACE('',(#935,#505,#506,#507,#508,#509),#643,.F.);
#5436=ADVANCED_FACE('',(#936,#510),#244,.F.);
#5437=ADVANCED_FACE('',(#937),#5224,.F.);
#5438=ADVANCED_FACE('',(#938),#5225,.T.);
#5439=ADVANCED_FACE('',(#939,#511),#644,.T.);
#5440=ADVANCED_FACE('',(#940,#512),#645,.F.);
#5441=ADVANCED_FACE('',(#941),#646,.F.);
#5442=ADVANCED_FACE('',(#942),#647,.F.);
#5443=ADVANCED_FACE('',(#943),#648,.F.);
#5444=ADVANCED_FACE('',(#944),#649,.F.);
#5445=ADVANCED_FACE('',(#945),#650,.F.);
#5446=ADVANCED_FACE('',(#946),#651,.F.);
#5447=ADVANCED_FACE('',(#947),#652,.F.);
#5448=ADVANCED_FACE('',(#948),#653,.F.);
#5449=ADVANCED_FACE('',(#949,#513),#654,.T.);
#5450=ADVANCED_FACE('',(#950),#5226,.T.);
#5451=ADVANCED_FACE('',(#951),#655,.F.);
#5452=ADVANCED_FACE('',(#952),#656,.T.);
#5453=ADVANCED_FACE('',(#953),#266,.T.);
#5454=ADVANCED_FACE('',(#954),#5227,.T.);
#5455=ADVANCED_FACE('',(#955),#267,.T.);
#5456=ADVANCED_FACE('',(#956,#514),#657,.T.);
#5457=ADVANCED_FACE('',(#957),#268,.T.);
#5458=ADVANCED_FACE('',(#958),#5228,.T.);
#5459=ADVANCED_FACE('',(#959),#269,.F.);
#5460=ADVANCED_FACE('',(#960),#5229,.F.);
#5461=ADVANCED_FACE('',(#961,#515),#658,.T.);
#5462=ADVANCED_FACE('',(#962),#5230,.T.);
#5463=ADVANCED_FACE('',(#963,#516),#659,.F.);
#5464=ADVANCED_FACE('',(#964),#270,.T.);
#5465=ADVANCED_FACE('',(#965),#271,.T.);
#5466=ADVANCED_FACE('',(#966),#660,.T.);
#5467=ADVANCED_FACE('',(#967),#661,.T.);
#5468=ADVANCED_FACE('',(#968),#662,.T.);
#5469=ADVANCED_FACE('',(#969),#5231,.F.);
#5470=ADVANCED_FACE('',(#970),#663,.T.);
#5471=ADVANCED_FACE('',(#971),#664,.T.);
#5472=ADVANCED_FACE('',(#972),#665,.T.);
#5473=ADVANCED_FACE('',(#973,#517),#666,.T.);
#5474=ADVANCED_FACE('',(#974,#518),#667,.F.);
#5475=ADVANCED_FACE('',(#975,#519),#668,.F.);
#5476=ADVANCED_FACE('',(#976,#520),#669,.T.);
#5477=ADVANCED_FACE('',(#977),#670,.T.);
#5478=ADVANCED_FACE('',(#978),#671,.T.);
#5479=ADVANCED_FACE('',(#979),#672,.T.);
#5480=ADVANCED_FACE('',(#980),#673,.T.);
#5481=ADVANCED_FACE('',(#981),#674,.T.);
#5482=ADVANCED_FACE('',(#982),#675,.T.);
#5483=ADVANCED_FACE('',(#983),#5232,.T.);
#5484=ADVANCED_FACE('',(#984,#521),#676,.T.);
#5485=ADVANCED_FACE('',(#985),#272,.T.);
#5486=ADVANCED_FACE('',(#986),#5233,.T.);
#5487=ADVANCED_FACE('',(#987),#273,.T.);
#5488=ADVANCED_FACE('',(#988,#522),#677,.T.);
#5489=ADVANCED_FACE('',(#989),#5234,.F.);
#5490=ADVANCED_FACE('',(#990),#5235,.F.);
#5491=ADVANCED_FACE('',(#991),#5236,.T.);
#5492=ADVANCED_FACE('',(#992,#523),#678,.T.);
#5493=ADVANCED_FACE('',(#993,#524),#679,.F.);
#5494=ADVANCED_FACE('',(#994),#680,.T.);
#5495=ADVANCED_FACE('',(#995),#274,.T.);
#5496=ADVANCED_FACE('',(#996),#5237,.T.);
#5497=ADVANCED_FACE('',(#997),#275,.T.);
#5498=ADVANCED_FACE('',(#998,#525),#681,.T.);
#5499=ADVANCED_FACE('',(#999),#276,.T.);
#5500=ADVANCED_FACE('',(#1000),#5238,.T.);
#5501=ADVANCED_FACE('',(#1001),#277,.T.);
#5502=ADVANCED_FACE('',(#1002),#682,.T.);
#5503=ADVANCED_FACE('',(#1003),#683,.F.);
#5504=ADVANCED_FACE('',(#1004),#684,.F.);
#5505=ADVANCED_FACE('',(#1005),#685,.F.);
#5506=ADVANCED_FACE('',(#1006),#686,.F.);
#5507=ADVANCED_FACE('',(#1007),#687,.F.);
#5508=ADVANCED_FACE('',(#1008),#688,.F.);
#5509=ADVANCED_FACE('',(#1009),#689,.F.);
#5510=ADVANCED_FACE('',(#1010),#690,.F.);
#5511=ADVANCED_FACE('',(#1011),#5239,.T.);
#5512=ADVANCED_FACE('',(#1012),#691,.T.);
#5513=ADVANCED_FACE('',(#1013),#692,.F.);
#5514=ADVANCED_FACE('',(#1014),#693,.F.);
#5515=ADVANCED_FACE('',(#1015),#694,.F.);
#5516=ADVANCED_FACE('',(#1016),#695,.F.);
#5517=ADVANCED_FACE('',(#1017),#696,.F.);
#5518=ADVANCED_FACE('',(#1018),#697,.T.);
#5519=ADVANCED_FACE('',(#1019),#5240,.F.);
#5520=ADVANCED_FACE('',(#1020,#526,#527),#245,.T.);
#5521=ADVANCED_FACE('',(#1021),#5241,.F.);
#5522=ADVANCED_FACE('',(#1022),#698,.T.);
#5523=ADVANCED_FACE('',(#1023),#699,.F.);
#5524=ADVANCED_FACE('',(#1024),#700,.F.);
#5525=ADVANCED_FACE('',(#1025),#701,.F.);
#5526=ADVANCED_FACE('',(#1026),#702,.F.);
#5527=ADVANCED_FACE('',(#1027),#703,.T.);
#5528=ADVANCED_FACE('',(#1028),#704,.T.);
#5529=ADVANCED_FACE('',(#1029),#705,.T.);
#5530=ADVANCED_FACE('',(#1030),#706,.T.);
#5531=ADVANCED_FACE('',(#1031,#528),#707,.T.);
#5532=ADVANCED_FACE('',(#1032),#708,.T.);
#5533=ADVANCED_FACE('',(#1033),#709,.T.);
#5534=ADVANCED_FACE('',(#1034),#710,.T.);
#5535=ADVANCED_FACE('',(#1035),#711,.T.);
#5536=ADVANCED_FACE('',(#1036),#712,.T.);
#5537=ADVANCED_FACE('',(#1037),#713,.T.);
#5538=ADVANCED_FACE('',(#1038),#714,.T.);
#5539=ADVANCED_FACE('',(#1039),#715,.T.);
#5540=ADVANCED_FACE('',(#1040),#716,.F.);
#5541=ADVANCED_FACE('',(#1041),#5242,.T.);
#5542=ADVANCED_FACE('',(#1042,#529),#717,.F.);
#5543=ADVANCED_FACE('',(#1043),#718,.F.);
#5544=ADVANCED_FACE('',(#1044),#719,.F.);
#5545=ADVANCED_FACE('',(#1045),#720,.F.);
#5546=ADVANCED_FACE('',(#1046),#721,.F.);
#5547=ADVANCED_FACE('',(#1047),#722,.T.);
#5548=ADVANCED_FACE('',(#1048),#723,.T.);
#5549=ADVANCED_FACE('',(#1049),#724,.T.);
#5550=ADVANCED_FACE('',(#1050),#725,.T.);
#5551=ADVANCED_FACE('',(#1051,#530),#726,.T.);
#5552=ADVANCED_FACE('',(#1052,#531),#727,.F.);
#5553=ADVANCED_FACE('',(#1053),#5243,.F.);
#5554=ADVANCED_FACE('',(#1054),#5244,.T.);
#5555=ADVANCED_FACE('',(#1055,#532),#728,.T.);
#5556=ADVANCED_FACE('',(#1056,#533),#729,.F.);
#5557=ADVANCED_FACE('',(#1057),#730,.T.);
#5558=ADVANCED_FACE('',(#1058),#731,.T.);
#5559=ADVANCED_FACE('',(#1059),#732,.T.);
#5560=ADVANCED_FACE('',(#1060),#733,.T.);
#5561=ADVANCED_FACE('',(#1061),#734,.T.);
#5562=ADVANCED_FACE('',(#1062),#735,.F.);
#5563=ADVANCED_FACE('',(#1063),#736,.F.);
#5564=ADVANCED_FACE('',(#1064),#737,.F.);
#5565=ADVANCED_FACE('',(#1065),#738,.F.);
#5566=ADVANCED_FACE('',(#1066),#739,.F.);
#5567=ADVANCED_FACE('',(#1067),#740,.F.);
#5568=ADVANCED_FACE('',(#1068),#741,.F.);
#5569=ADVANCED_FACE('',(#1069),#742,.F.);
#5570=ADVANCED_FACE('',(#1070),#743,.F.);
#5571=ADVANCED_FACE('',(#1071),#744,.F.);
#5572=ADVANCED_FACE('',(#1072),#745,.T.);
#5573=ADVANCED_FACE('',(#1073),#278,.T.);
#5574=ADVANCED_FACE('',(#1074),#5245,.T.);
#5575=ADVANCED_FACE('',(#1075),#279,.T.);
#5576=ADVANCED_FACE('',(#1076,#534),#746,.T.);
#5577=ADVANCED_FACE('',(#1077),#280,.T.);
#5578=ADVANCED_FACE('',(#1078),#5246,.T.);
#5579=CLOSED_SHELL('',(#5247,#5248,#5249,#5250,#5251,#5252,#5253,#5254,
#5255,#5256,#5257,#5258,#5259,#5260,#5261,#5262,#5263,#5264,#5265,#5266,
#5267,#5268,#5269,#5270,#5271,#5272,#5273,#5274,#5275,#5276,#5277,#5278,
#5279,#5280,#5281,#5282,#5283,#5284,#5285,#5286,#5287,#5288,#5289,#5290,
#5291,#5292,#5293,#5294,#5295,#5296,#5297));
#5580=CLOSED_SHELL('',(#5298,#5299,#5300,#5301,#5302,#5303,#5304,#5305,
#5306,#5307));
#5581=CLOSED_SHELL('',(#5308,#5309,#5310,#5311,#5312,#5313,#5314,#5315,
#5316,#5317,#5318,#5319,#5320,#5321,#5322));
#5582=CLOSED_SHELL('',(#5323,#5324,#5325,#5326,#5327,#5328,#5329,#5330,
#5331,#5332,#5333,#5334,#5335,#5336,#5337));
#5583=CLOSED_SHELL('',(#5338,#5339,#5340,#5341,#5342,#5343,#5344,#5345,
#5346,#5347,#5348,#5349));
#5584=CLOSED_SHELL('',(#5350,#5351,#5352,#5353,#5354,#5355,#5356,#5357,
#5358,#5359,#5360,#5361,#5362,#5363,#5364,#5365,#5366,#5367,#5368,#5369,
#5370));
#5585=CLOSED_SHELL('',(#5371,#5372,#5373,#5374,#5375,#5376,#5377,#5378,
#5379,#5380,#5381,#5382,#5383,#5384,#5385,#5386,#5387,#5388,#5389,#5390,
#5391));
#5586=CLOSED_SHELL('',(#5392,#5393,#5394,#5395,#5396,#5397,#5398,#5399,
#5400,#5401,#5402,#5403,#5404,#5405,#5406,#5407));
#5587=CLOSED_SHELL('',(#5408,#5409,#5410,#5411,#5412,#5413));
#5588=CLOSED_SHELL('',(#5414));
#5589=CLOSED_SHELL('',(#5415,#5416,#5417,#5418,#5419,#5420));
#5590=CLOSED_SHELL('',(#5421,#5422,#5423,#5424,#5425,#5426,#5427,#5428,
#5429,#5430,#5431,#5432,#5433,#5434,#5435));
#5591=CLOSED_SHELL('',(#5436,#5437,#5438,#5439,#5440));
#5592=CLOSED_SHELL('',(#5441,#5442,#5443,#5444,#5445,#5446,#5447,#5448));
#5593=CLOSED_SHELL('',(#5449,#5450,#5451,#5452,#5453,#5454,#5455,#5456,
#5457,#5458));
#5594=CLOSED_SHELL('',(#5459,#5460,#5461,#5462,#5463));
#5595=CLOSED_SHELL('',(#5464,#5465,#5466,#5467,#5468,#5469,#5470,#5471,
#5472,#5473,#5474));
#5596=CLOSED_SHELL('',(#5475,#5476,#5477,#5478,#5479,#5480,#5481,#5482,
#5483,#5484,#5485,#5486,#5487,#5488,#5489));
#5597=CLOSED_SHELL('',(#5490,#5491,#5492,#5493));
#5598=CLOSED_SHELL('',(#5494,#5495,#5496,#5497,#5498,#5499,#5500,#5501,
#5502));
#5599=CLOSED_SHELL('',(#5503,#5504,#5505,#5506,#5507,#5508,#5509,#5510));
#5600=CLOSED_SHELL('',(#5511,#5512,#5513));
#5601=CLOSED_SHELL('',(#5514,#5515,#5516,#5517,#5518,#5519,#5520));
#5602=CLOSED_SHELL('',(#5521,#5522,#5523,#5524,#5525,#5526,#5527,#5528,
#5529,#5530,#5531,#5532,#5533,#5534,#5535,#5536,#5537,#5538,#5539,#5540,
#5541,#5542));
#5603=CLOSED_SHELL('',(#5543,#5544,#5545,#5546,#5547,#5548,#5549,#5550,
#5551,#5552));
#5604=CLOSED_SHELL('',(#5553,#5554,#5555,#5556));
#5605=CLOSED_SHELL('',(#5557,#5558,#5559,#5560,#5561,#5562));
#5606=CLOSED_SHELL('',(#5563,#5564,#5565,#5566,#5567,#5568,#5569,#5570));
#5607=CLOSED_SHELL('',(#5571,#5572,#5573,#5574,#5575,#5576,#5577,#5578));
#5608=DERIVED_UNIT_ELEMENT(#5660,1.);
#5609=DERIVED_UNIT_ELEMENT(#10121,-3.);
#5610=DERIVED_UNIT_ELEMENT(#5660,1.);
#5611=DERIVED_UNIT_ELEMENT(#10121,-3.);
#5612=DERIVED_UNIT_ELEMENT(#5660,1.);
#5613=DERIVED_UNIT_ELEMENT(#10121,-3.);
#5614=DERIVED_UNIT_ELEMENT(#5660,1.);
#5615=DERIVED_UNIT_ELEMENT(#10121,-3.);
#5616=DERIVED_UNIT_ELEMENT(#5660,1.);
#5617=DERIVED_UNIT_ELEMENT(#10121,-3.);
#5618=DERIVED_UNIT_ELEMENT(#5660,1.);
#5619=DERIVED_UNIT_ELEMENT(#10121,-3.);
#5620=DERIVED_UNIT_ELEMENT(#5660,1.);
#5621=DERIVED_UNIT_ELEMENT(#10121,-3.);
#5622=DERIVED_UNIT_ELEMENT(#5660,1.);
#5623=DERIVED_UNIT_ELEMENT(#10121,-3.);
#5624=DERIVED_UNIT_ELEMENT(#5660,1.);
#5625=DERIVED_UNIT_ELEMENT(#10121,-3.);
#5626=DERIVED_UNIT_ELEMENT(#5660,1.);
#5627=DERIVED_UNIT_ELEMENT(#10121,-3.);
#5628=DERIVED_UNIT_ELEMENT(#5660,1.);
#5629=DERIVED_UNIT_ELEMENT(#10121,-3.);
#5630=DERIVED_UNIT_ELEMENT(#5660,1.);
#5631=DERIVED_UNIT_ELEMENT(#10121,-3.);
#5632=DERIVED_UNIT_ELEMENT(#5660,1.);
#5633=DERIVED_UNIT_ELEMENT(#10121,-3.);
#5634=DERIVED_UNIT_ELEMENT(#5660,1.);
#5635=DERIVED_UNIT_ELEMENT(#10121,-3.);
#5636=DERIVED_UNIT_ELEMENT(#5660,1.);
#5637=DERIVED_UNIT_ELEMENT(#10121,-3.);
#5638=DERIVED_UNIT_ELEMENT(#5660,1.);
#5639=DERIVED_UNIT_ELEMENT(#10121,-3.);
#5640=DERIVED_UNIT_ELEMENT(#5660,1.);
#5641=DERIVED_UNIT_ELEMENT(#10121,-3.);
#5642=DERIVED_UNIT_ELEMENT(#5660,1.);
#5643=DERIVED_UNIT_ELEMENT(#10121,-3.);
#5644=DERIVED_UNIT_ELEMENT(#5660,1.);
#5645=DERIVED_UNIT_ELEMENT(#10121,-3.);
#5646=DERIVED_UNIT_ELEMENT(#5660,1.);
#5647=DERIVED_UNIT_ELEMENT(#10121,-3.);
#5648=DERIVED_UNIT_ELEMENT(#5660,1.);
#5649=DERIVED_UNIT_ELEMENT(#10121,-3.);
#5650=DERIVED_UNIT_ELEMENT(#5660,1.);
#5651=DERIVED_UNIT_ELEMENT(#10121,-3.);
#5652=DERIVED_UNIT_ELEMENT(#5660,1.);
#5653=DERIVED_UNIT_ELEMENT(#10121,-3.);
#5654=DERIVED_UNIT_ELEMENT(#5660,1.);
#5655=DERIVED_UNIT_ELEMENT(#10121,-3.);
#5656=DERIVED_UNIT_ELEMENT(#5660,1.);
#5657=DERIVED_UNIT_ELEMENT(#10121,-3.);
#5658=DERIVED_UNIT_ELEMENT(#5660,1.);
#5659=DERIVED_UNIT_ELEMENT(#10121,-3.);
#5660=(
MASS_UNIT()
NAMED_UNIT(*)
SI_UNIT(.KILO.,.GRAM.)
);
#5661=DERIVED_UNIT((#5608,#5609));
#5662=DERIVED_UNIT((#5610,#5611));
#5663=DERIVED_UNIT((#5612,#5613));
#5664=DERIVED_UNIT((#5614,#5615));
#5665=DERIVED_UNIT((#5616,#5617));
#5666=DERIVED_UNIT((#5618,#5619));
#5667=DERIVED_UNIT((#5620,#5621));
#5668=DERIVED_UNIT((#5622,#5623));
#5669=DERIVED_UNIT((#5624,#5625));
#5670=DERIVED_UNIT((#5626,#5627));
#5671=DERIVED_UNIT((#5628,#5629));
#5672=DERIVED_UNIT((#5630,#5631));
#5673=DERIVED_UNIT((#5632,#5633));
#5674=DERIVED_UNIT((#5634,#5635));
#5675=DERIVED_UNIT((#5636,#5637));
#5676=DERIVED_UNIT((#5638,#5639));
#5677=DERIVED_UNIT((#5640,#5641));
#5678=DERIVED_UNIT((#5642,#5643));
#5679=DERIVED_UNIT((#5644,#5645));
#5680=DERIVED_UNIT((#5646,#5647));
#5681=DERIVED_UNIT((#5648,#5649));
#5682=DERIVED_UNIT((#5650,#5651));
#5683=DERIVED_UNIT((#5652,#5653));
#5684=DERIVED_UNIT((#5654,#5655));
#5685=DERIVED_UNIT((#5656,#5657));
#5686=DERIVED_UNIT((#5658,#5659));
#5687=MEASURE_REPRESENTATION_ITEM('density measure',
POSITIVE_RATIO_MEASURE(7850.),#5661);
#5688=MEASURE_REPRESENTATION_ITEM('density measure',
POSITIVE_RATIO_MEASURE(7850.),#5662);
#5689=MEASURE_REPRESENTATION_ITEM('density measure',
POSITIVE_RATIO_MEASURE(7850.),#5663);
#5690=MEASURE_REPRESENTATION_ITEM('density measure',
POSITIVE_RATIO_MEASURE(7850.),#5664);
#5691=MEASURE_REPRESENTATION_ITEM('density measure',
POSITIVE_RATIO_MEASURE(7850.),#5665);
#5692=MEASURE_REPRESENTATION_ITEM('density measure',
POSITIVE_RATIO_MEASURE(7850.),#5666);
#5693=MEASURE_REPRESENTATION_ITEM('density measure',
POSITIVE_RATIO_MEASURE(7850.),#5667);
#5694=MEASURE_REPRESENTATION_ITEM('density measure',
POSITIVE_RATIO_MEASURE(7850.),#5668);
#5695=MEASURE_REPRESENTATION_ITEM('density measure',
POSITIVE_RATIO_MEASURE(7850.),#5669);
#5696=MEASURE_REPRESENTATION_ITEM('density measure',
POSITIVE_RATIO_MEASURE(7850.),#5670);
#5697=MEASURE_REPRESENTATION_ITEM('density measure',
POSITIVE_RATIO_MEASURE(7850.),#5671);
#5698=MEASURE_REPRESENTATION_ITEM('density measure',
POSITIVE_RATIO_MEASURE(7850.),#5672);
#5699=MEASURE_REPRESENTATION_ITEM('density measure',
POSITIVE_RATIO_MEASURE(7850.),#5673);
#5700=MEASURE_REPRESENTATION_ITEM('density measure',
POSITIVE_RATIO_MEASURE(7850.),#5674);
#5701=MEASURE_REPRESENTATION_ITEM('density measure',
POSITIVE_RATIO_MEASURE(7850.),#5675);
#5702=MEASURE_REPRESENTATION_ITEM('density measure',
POSITIVE_RATIO_MEASURE(7850.),#5676);
#5703=MEASURE_REPRESENTATION_ITEM('density measure',
POSITIVE_RATIO_MEASURE(7850.),#5677);
#5704=MEASURE_REPRESENTATION_ITEM('density measure',
POSITIVE_RATIO_MEASURE(7850.),#5678);
#5705=MEASURE_REPRESENTATION_ITEM('density measure',
POSITIVE_RATIO_MEASURE(7850.),#5679);
#5706=MEASURE_REPRESENTATION_ITEM('density measure',
POSITIVE_RATIO_MEASURE(7850.),#5680);
#5707=MEASURE_REPRESENTATION_ITEM('density measure',
POSITIVE_RATIO_MEASURE(7850.),#5681);
#5708=MEASURE_REPRESENTATION_ITEM('density measure',
POSITIVE_RATIO_MEASURE(7850.),#5682);
#5709=MEASURE_REPRESENTATION_ITEM('density measure',
POSITIVE_RATIO_MEASURE(7850.),#5683);
#5710=MEASURE_REPRESENTATION_ITEM('density measure',
POSITIVE_RATIO_MEASURE(7850.),#5684);
#5711=MEASURE_REPRESENTATION_ITEM('density measure',
POSITIVE_RATIO_MEASURE(7850.),#5685);
#5712=MEASURE_REPRESENTATION_ITEM('density measure',
POSITIVE_RATIO_MEASURE(7850.),#5686);
#5713=PROPERTY_DEFINITION_REPRESENTATION(#5843,#5765);
#5714=PROPERTY_DEFINITION_REPRESENTATION(#5844,#5766);
#5715=PROPERTY_DEFINITION_REPRESENTATION(#5845,#5767);
#5716=PROPERTY_DEFINITION_REPRESENTATION(#5846,#5768);
#5717=PROPERTY_DEFINITION_REPRESENTATION(#5847,#5769);
#5718=PROPERTY_DEFINITION_REPRESENTATION(#5848,#5770);
#5719=PROPERTY_DEFINITION_REPRESENTATION(#5849,#5771);
#5720=PROPERTY_DEFINITION_REPRESENTATION(#5850,#5772);
#5721=PROPERTY_DEFINITION_REPRESENTATION(#5851,#5773);
#5722=PROPERTY_DEFINITION_REPRESENTATION(#5852,#5774);
#5723=PROPERTY_DEFINITION_REPRESENTATION(#5853,#5775);
#5724=PROPERTY_DEFINITION_REPRESENTATION(#5854,#5776);
#5725=PROPERTY_DEFINITION_REPRESENTATION(#5855,#5777);
#5726=PROPERTY_DEFINITION_REPRESENTATION(#5856,#5778);
#5727=PROPERTY_DEFINITION_REPRESENTATION(#5857,#5779);
#5728=PROPERTY_DEFINITION_REPRESENTATION(#5858,#5780);
#5729=PROPERTY_DEFINITION_REPRESENTATION(#5859,#5781);
#5730=PROPERTY_DEFINITION_REPRESENTATION(#5860,#5782);
#5731=PROPERTY_DEFINITION_REPRESENTATION(#5861,#5783);
#5732=PROPERTY_DEFINITION_REPRESENTATION(#5862,#5784);
#5733=PROPERTY_DEFINITION_REPRESENTATION(#5863,#5785);
#5734=PROPERTY_DEFINITION_REPRESENTATION(#5864,#5786);
#5735=PROPERTY_DEFINITION_REPRESENTATION(#5865,#5787);
#5736=PROPERTY_DEFINITION_REPRESENTATION(#5866,#5788);
#5737=PROPERTY_DEFINITION_REPRESENTATION(#5867,#5789);
#5738=PROPERTY_DEFINITION_REPRESENTATION(#5868,#5790);
#5739=PROPERTY_DEFINITION_REPRESENTATION(#5869,#5791);
#5740=PROPERTY_DEFINITION_REPRESENTATION(#5870,#5792);
#5741=PROPERTY_DEFINITION_REPRESENTATION(#5871,#5793);
#5742=PROPERTY_DEFINITION_REPRESENTATION(#5872,#5794);
#5743=PROPERTY_DEFINITION_REPRESENTATION(#5873,#5795);
#5744=PROPERTY_DEFINITION_REPRESENTATION(#5874,#5796);
#5745=PROPERTY_DEFINITION_REPRESENTATION(#5875,#5797);
#5746=PROPERTY_DEFINITION_REPRESENTATION(#5876,#5798);
#5747=PROPERTY_DEFINITION_REPRESENTATION(#5877,#5799);
#5748=PROPERTY_DEFINITION_REPRESENTATION(#5878,#5800);
#5749=PROPERTY_DEFINITION_REPRESENTATION(#5879,#5801);
#5750=PROPERTY_DEFINITION_REPRESENTATION(#5880,#5802);
#5751=PROPERTY_DEFINITION_REPRESENTATION(#5881,#5803);
#5752=PROPERTY_DEFINITION_REPRESENTATION(#5882,#5804);
#5753=PROPERTY_DEFINITION_REPRESENTATION(#5883,#5805);
#5754=PROPERTY_DEFINITION_REPRESENTATION(#5884,#5806);
#5755=PROPERTY_DEFINITION_REPRESENTATION(#5885,#5807);
#5756=PROPERTY_DEFINITION_REPRESENTATION(#5886,#5808);
#5757=PROPERTY_DEFINITION_REPRESENTATION(#5887,#5809);
#5758=PROPERTY_DEFINITION_REPRESENTATION(#5888,#5810);
#5759=PROPERTY_DEFINITION_REPRESENTATION(#5889,#5811);
#5760=PROPERTY_DEFINITION_REPRESENTATION(#5890,#5812);
#5761=PROPERTY_DEFINITION_REPRESENTATION(#5891,#5813);
#5762=PROPERTY_DEFINITION_REPRESENTATION(#5892,#5814);
#5763=PROPERTY_DEFINITION_REPRESENTATION(#5893,#5815);
#5764=PROPERTY_DEFINITION_REPRESENTATION(#5894,#5816);
#5765=REPRESENTATION('material name',(#5817),#10091);
#5766=REPRESENTATION('density',(#5687),#10091);
#5767=REPRESENTATION('material name',(#5818),#10092);
#5768=REPRESENTATION('density',(#5688),#10092);
#5769=REPRESENTATION('material name',(#5819),#10093);
#5770=REPRESENTATION('density',(#5689),#10093);
#5771=REPRESENTATION('material name',(#5820),#10094);
#5772=REPRESENTATION('density',(#5690),#10094);
#5773=REPRESENTATION('material name',(#5821),#10095);
#5774=REPRESENTATION('density',(#5691),#10095);
#5775=REPRESENTATION('material name',(#5822),#10097);
#5776=REPRESENTATION('density',(#5692),#10097);
#5777=REPRESENTATION('material name',(#5823),#10098);
#5778=REPRESENTATION('density',(#5693),#10098);
#5779=REPRESENTATION('material name',(#5824),#10099);
#5780=REPRESENTATION('density',(#5694),#10099);
#5781=REPRESENTATION('material name',(#5825),#10100);
#5782=REPRESENTATION('density',(#5695),#10100);
#5783=REPRESENTATION('material name',(#5826),#10101);
#5784=REPRESENTATION('density',(#5696),#10101);
#5785=REPRESENTATION('material name',(#5827),#10102);
#5786=REPRESENTATION('density',(#5697),#10102);
#5787=REPRESENTATION('material name',(#5828),#10103);
#5788=REPRESENTATION('density',(#5698),#10103);
#5789=REPRESENTATION('material name',(#5829),#10104);
#5790=REPRESENTATION('density',(#5699),#10104);
#5791=REPRESENTATION('material name',(#5830),#10105);
#5792=REPRESENTATION('density',(#5700),#10105);
#5793=REPRESENTATION('material name',(#5831),#10106);
#5794=REPRESENTATION('density',(#5701),#10106);
#5795=REPRESENTATION('material name',(#5832),#10107);
#5796=REPRESENTATION('density',(#5702),#10107);
#5797=REPRESENTATION('material name',(#5833),#10108);
#5798=REPRESENTATION('density',(#5703),#10108);
#5799=REPRESENTATION('material name',(#5834),#10109);
#5800=REPRESENTATION('density',(#5704),#10109);
#5801=REPRESENTATION('material name',(#5835),#10110);
#5802=REPRESENTATION('density',(#5705),#10110);
#5803=REPRESENTATION('material name',(#5836),#10111);
#5804=REPRESENTATION('density',(#5706),#10111);
#5805=REPRESENTATION('material name',(#5837),#10113);
#5806=REPRESENTATION('density',(#5707),#10113);
#5807=REPRESENTATION('material name',(#5838),#10114);
#5808=REPRESENTATION('density',(#5708),#10114);
#5809=REPRESENTATION('material name',(#5839),#10115);
#5810=REPRESENTATION('density',(#5709),#10115);
#5811=REPRESENTATION('material name',(#5840),#10116);
#5812=REPRESENTATION('density',(#5710),#10116);
#5813=REPRESENTATION('material name',(#5841),#10117);
#5814=REPRESENTATION('density',(#5711),#10117);
#5815=REPRESENTATION('material name',(#5842),#10118);
#5816=REPRESENTATION('density',(#5712),#10118);
#5817=DESCRIPTIVE_REPRESENTATION_ITEM('Steel','Steel');
#5818=DESCRIPTIVE_REPRESENTATION_ITEM('Steel','Steel');
#5819=DESCRIPTIVE_REPRESENTATION_ITEM('Steel','Steel');
#5820=DESCRIPTIVE_REPRESENTATION_ITEM('Steel','Steel');
#5821=DESCRIPTIVE_REPRESENTATION_ITEM('Steel','Steel');
#5822=DESCRIPTIVE_REPRESENTATION_ITEM('Steel','Steel');
#5823=DESCRIPTIVE_REPRESENTATION_ITEM('Steel','Steel');
#5824=DESCRIPTIVE_REPRESENTATION_ITEM('Steel','Steel');
#5825=DESCRIPTIVE_REPRESENTATION_ITEM('Steel','Steel');
#5826=DESCRIPTIVE_REPRESENTATION_ITEM('Steel','Steel');
#5827=DESCRIPTIVE_REPRESENTATION_ITEM('Steel','Steel');
#5828=DESCRIPTIVE_REPRESENTATION_ITEM('Steel','Steel');
#5829=DESCRIPTIVE_REPRESENTATION_ITEM('Steel','Steel');
#5830=DESCRIPTIVE_REPRESENTATION_ITEM('Steel','Steel');
#5831=DESCRIPTIVE_REPRESENTATION_ITEM('Steel','Steel');
#5832=DESCRIPTIVE_REPRESENTATION_ITEM('Steel','Steel');
#5833=DESCRIPTIVE_REPRESENTATION_ITEM('Steel','Steel');
#5834=DESCRIPTIVE_REPRESENTATION_ITEM('Steel','Steel');
#5835=DESCRIPTIVE_REPRESENTATION_ITEM('Steel','Steel');
#5836=DESCRIPTIVE_REPRESENTATION_ITEM('Steel','Steel');
#5837=DESCRIPTIVE_REPRESENTATION_ITEM('Steel','Steel');
#5838=DESCRIPTIVE_REPRESENTATION_ITEM('Steel','Steel');
#5839=DESCRIPTIVE_REPRESENTATION_ITEM('Steel','Steel');
#5840=DESCRIPTIVE_REPRESENTATION_ITEM('Steel','Steel');
#5841=DESCRIPTIVE_REPRESENTATION_ITEM('Steel','Steel');
#5842=DESCRIPTIVE_REPRESENTATION_ITEM('Steel','Steel');
#5843=PROPERTY_DEFINITION('material property','material name',#10273);
#5844=PROPERTY_DEFINITION('material property','density of part',#10273);
#5845=PROPERTY_DEFINITION('material property','material name',#10274);
#5846=PROPERTY_DEFINITION('material property','density of part',#10274);
#5847=PROPERTY_DEFINITION('material property','material name',#10275);
#5848=PROPERTY_DEFINITION('material property','density of part',#10275);
#5849=PROPERTY_DEFINITION('material property','material name',#10276);
#5850=PROPERTY_DEFINITION('material property','density of part',#10276);
#5851=PROPERTY_DEFINITION('material property','material name',#10277);
#5852=PROPERTY_DEFINITION('material property','density of part',#10277);
#5853=PROPERTY_DEFINITION('material property','material name',#10279);
#5854=PROPERTY_DEFINITION('material property','density of part',#10279);
#5855=PROPERTY_DEFINITION('material property','material name',#10280);
#5856=PROPERTY_DEFINITION('material property','density of part',#10280);
#5857=PROPERTY_DEFINITION('material property','material name',#10281);
#5858=PROPERTY_DEFINITION('material property','density of part',#10281);
#5859=PROPERTY_DEFINITION('material property','material name',#10282);
#5860=PROPERTY_DEFINITION('material property','density of part',#10282);
#5861=PROPERTY_DEFINITION('material property','material name',#10283);
#5862=PROPERTY_DEFINITION('material property','density of part',#10283);
#5863=PROPERTY_DEFINITION('material property','material name',#10284);
#5864=PROPERTY_DEFINITION('material property','density of part',#10284);
#5865=PROPERTY_DEFINITION('material property','material name',#10285);
#5866=PROPERTY_DEFINITION('material property','density of part',#10285);
#5867=PROPERTY_DEFINITION('material property','material name',#10286);
#5868=PROPERTY_DEFINITION('material property','density of part',#10286);
#5869=PROPERTY_DEFINITION('material property','material name',#10287);
#5870=PROPERTY_DEFINITION('material property','density of part',#10287);
#5871=PROPERTY_DEFINITION('material property','material name',#10288);
#5872=PROPERTY_DEFINITION('material property','density of part',#10288);
#5873=PROPERTY_DEFINITION('material property','material name',#10289);
#5874=PROPERTY_DEFINITION('material property','density of part',#10289);
#5875=PROPERTY_DEFINITION('material property','material name',#10290);
#5876=PROPERTY_DEFINITION('material property','density of part',#10290);
#5877=PROPERTY_DEFINITION('material property','material name',#10291);
#5878=PROPERTY_DEFINITION('material property','density of part',#10291);
#5879=PROPERTY_DEFINITION('material property','material name',#10292);
#5880=PROPERTY_DEFINITION('material property','density of part',#10292);
#5881=PROPERTY_DEFINITION('material property','material name',#10293);
#5882=PROPERTY_DEFINITION('material property','density of part',#10293);
#5883=PROPERTY_DEFINITION('material property','material name',#10295);
#5884=PROPERTY_DEFINITION('material property','density of part',#10295);
#5885=PROPERTY_DEFINITION('material property','material name',#10296);
#5886=PROPERTY_DEFINITION('material property','density of part',#10296);
#5887=PROPERTY_DEFINITION('material property','material name',#10297);
#5888=PROPERTY_DEFINITION('material property','density of part',#10297);
#5889=PROPERTY_DEFINITION('material property','material name',#10298);
#5890=PROPERTY_DEFINITION('material property','density of part',#10298);
#5891=PROPERTY_DEFINITION('material property','material name',#10299);
#5892=PROPERTY_DEFINITION('material property','density of part',#10299);
#5893=PROPERTY_DEFINITION('material property','material name',#10300);
#5894=PROPERTY_DEFINITION('material property','density of part',#10300);
#5895=AXIS2_PLACEMENT_3D('',#8335,#6569,#6570);
#5896=AXIS2_PLACEMENT_3D('',#8336,#6571,#6572);
#5897=AXIS2_PLACEMENT_3D('',#8337,#6573,#6574);
#5898=AXIS2_PLACEMENT_3D('',#8338,#6575,#6576);
#5899=AXIS2_PLACEMENT_3D('',#8340,#6577,#6578);
#5900=AXIS2_PLACEMENT_3D('',#8343,#6580,#6581);
#5901=AXIS2_PLACEMENT_3D('',#8344,#6582,#6583);
#5902=AXIS2_PLACEMENT_3D('',#8345,#6584,#6585);
#5903=AXIS2_PLACEMENT_3D('',#8347,#6586,#6587);
#5904=AXIS2_PLACEMENT_3D('',#8350,#6589,#6590);
#5905=AXIS2_PLACEMENT_3D('',#8351,#6591,#6592);
#5906=AXIS2_PLACEMENT_3D('',#8352,#6593,#6594);
#5907=AXIS2_PLACEMENT_3D('',#8354,#6595,#6596);
#5908=AXIS2_PLACEMENT_3D('',#8357,#6598,#6599);
#5909=AXIS2_PLACEMENT_3D('',#8358,#6600,#6601);
#5910=AXIS2_PLACEMENT_3D('',#8360,#6602,#6603);
#5911=AXIS2_PLACEMENT_3D('',#8361,#6604,#6605);
#5912=AXIS2_PLACEMENT_3D('',#8363,#6606,#6607);
#5913=AXIS2_PLACEMENT_3D('',#8366,#6609,#6610);
#5914=AXIS2_PLACEMENT_3D('',#8367,#6611,#6612);
#5915=AXIS2_PLACEMENT_3D('',#8369,#6613,#6614);
#5916=AXIS2_PLACEMENT_3D('',#8370,#6615,#6616);
#5917=AXIS2_PLACEMENT_3D('',#8374,#6618,#6619);
#5918=AXIS2_PLACEMENT_3D('',#8375,#6620,#6621);
#5919=AXIS2_PLACEMENT_3D('',#8377,#6622,#6623);
#5920=AXIS2_PLACEMENT_3D('',#8378,#6624,#6625);
#5921=AXIS2_PLACEMENT_3D('',#8379,#6626,#6627);
#5922=AXIS2_PLACEMENT_3D('',#8382,#6628,#6629);
#5923=AXIS2_PLACEMENT_3D('',#8384,#6630,#6631);
#5924=AXIS2_PLACEMENT_3D('',#8385,#6632,#6633);
#5925=AXIS2_PLACEMENT_3D('',#8386,#6634,#6635);
#5926=AXIS2_PLACEMENT_3D('',#8388,#6636,#6637);
#5927=AXIS2_PLACEMENT_3D('',#8390,#6638,#6639);
#5928=AXIS2_PLACEMENT_3D('',#8391,#6640,#6641);
#5929=AXIS2_PLACEMENT_3D('',#8392,#6642,#6643);
#5930=AXIS2_PLACEMENT_3D('',#8394,#6644,#6645);
#5931=AXIS2_PLACEMENT_3D('',#8396,#6646,#6647);
#5932=AXIS2_PLACEMENT_3D('',#8397,#6648,#6649);
#5933=AXIS2_PLACEMENT_3D('',#8398,#6650,#6651);
#5934=AXIS2_PLACEMENT_3D('',#8400,#6653,#6654);
#5935=AXIS2_PLACEMENT_3D('',#8404,#6656,#6657);
#5936=AXIS2_PLACEMENT_3D('',#8428,#6660,#6661);
#5937=AXIS2_PLACEMENT_3D('',#8430,#6662,#6663);
#5938=AXIS2_PLACEMENT_3D('',#8433,#6665,#6666);
#5939=AXIS2_PLACEMENT_3D('',#8435,#6667,#6668);
#5940=AXIS2_PLACEMENT_3D('',#8455,#6671,#6672);
#5941=AXIS2_PLACEMENT_3D('',#8459,#6674,#6675);
#5942=AXIS2_PLACEMENT_3D('',#8483,#6678,#6679);
#5943=AXIS2_PLACEMENT_3D('',#8485,#6680,#6681);
#5944=AXIS2_PLACEMENT_3D('',#8488,#6683,#6684);
#5945=AXIS2_PLACEMENT_3D('',#8490,#6685,#6686);
#5946=AXIS2_PLACEMENT_3D('',#8510,#6689,#6690);
#5947=AXIS2_PLACEMENT_3D('',#8514,#6692,#6693);
#5948=AXIS2_PLACEMENT_3D('',#8538,#6696,#6697);
#5949=AXIS2_PLACEMENT_3D('',#8540,#6698,#6699);
#5950=AXIS2_PLACEMENT_3D('',#8543,#6701,#6702);
#5951=AXIS2_PLACEMENT_3D('',#8545,#6703,#6704);
#5952=AXIS2_PLACEMENT_3D('',#8565,#6707,#6708);
#5953=AXIS2_PLACEMENT_3D('',#8608,#6715,#6716);
#5954=AXIS2_PLACEMENT_3D('',#8611,#6718,#6719);
#5955=AXIS2_PLACEMENT_3D('',#8613,#6720,#6721);
#5956=AXIS2_PLACEMENT_3D('',#8616,#6723,#6724);
#5957=AXIS2_PLACEMENT_3D('',#8618,#6725,#6726);
#5958=AXIS2_PLACEMENT_3D('',#8621,#6728,#6729);
#5959=AXIS2_PLACEMENT_3D('',#8622,#6730,#6731);
#5960=AXIS2_PLACEMENT_3D('',#8623,#6732,#6733);
#5961=AXIS2_PLACEMENT_3D('',#8624,#6734,#6735);
#5962=AXIS2_PLACEMENT_3D('',#8626,#6736,#6737);
#5963=AXIS2_PLACEMENT_3D('',#8628,#6739,#6740);
#5964=AXIS2_PLACEMENT_3D('',#8629,#6741,#6742);
#5965=AXIS2_PLACEMENT_3D('',#8630,#6743,#6744);
#5966=AXIS2_PLACEMENT_3D('',#8631,#6745,#6746);
#5967=AXIS2_PLACEMENT_3D('',#8632,#6747,#6748);
#5968=AXIS2_PLACEMENT_3D('',#8633,#6749,#6750);
#5969=AXIS2_PLACEMENT_3D('',#8634,#6751,#6752);
#5970=AXIS2_PLACEMENT_3D('',#8635,#6753,#6754);
#5971=AXIS2_PLACEMENT_3D('',#8636,#6755,#6756);
#5972=AXIS2_PLACEMENT_3D('',#8637,#6757,#6758);
#5973=AXIS2_PLACEMENT_3D('',#8638,#6759,#6760);
#5974=AXIS2_PLACEMENT_3D('',#8639,#6761,#6762);
#5975=AXIS2_PLACEMENT_3D('',#8640,#6763,#6764);
#5976=AXIS2_PLACEMENT_3D('',#8641,#6765,#6766);
#5977=AXIS2_PLACEMENT_3D('',#8642,#6767,#6768);
#5978=AXIS2_PLACEMENT_3D('',#8644,#6769,#6770);
#5979=AXIS2_PLACEMENT_3D('',#8646,#6772,#6773);
#5980=AXIS2_PLACEMENT_3D('',#8647,#6774,#6775);
#5981=AXIS2_PLACEMENT_3D('',#8648,#6776,#6777);
#5982=AXIS2_PLACEMENT_3D('',#8649,#6778,#6779);
#5983=AXIS2_PLACEMENT_3D('',#8650,#6780,#6781);
#5984=AXIS2_PLACEMENT_3D('',#8651,#6782,#6783);
#5985=AXIS2_PLACEMENT_3D('',#8652,#6784,#6785);
#5986=AXIS2_PLACEMENT_3D('',#8653,#6786,#6787);
#5987=AXIS2_PLACEMENT_3D('',#8654,#6788,#6789);
#5988=AXIS2_PLACEMENT_3D('',#8655,#6790,#6791);
#5989=AXIS2_PLACEMENT_3D('',#8656,#6792,#6793);
#5990=AXIS2_PLACEMENT_3D('',#8657,#6794,#6795);
#5991=AXIS2_PLACEMENT_3D('',#8658,#6796,#6797);
#5992=AXIS2_PLACEMENT_3D('',#8659,#6798,#6799);
#5993=AXIS2_PLACEMENT_3D('',#8660,#6800,#6801);
#5994=AXIS2_PLACEMENT_3D('',#8662,#6802,#6803);
#5995=AXIS2_PLACEMENT_3D('',#8664,#6805,#6806);
#5996=AXIS2_PLACEMENT_3D('',#8665,#6807,#6808);
#5997=AXIS2_PLACEMENT_3D('',#8666,#6809,#6810);
#5998=AXIS2_PLACEMENT_3D('',#8667,#6811,#6812);
#5999=AXIS2_PLACEMENT_3D('',#8668,#6813,#6814);
#6000=AXIS2_PLACEMENT_3D('',#8669,#6815,#6816);
#6001=AXIS2_PLACEMENT_3D('',#8670,#6817,#6818);
#6002=AXIS2_PLACEMENT_3D('',#8671,#6819,#6820);
#6003=AXIS2_PLACEMENT_3D('',#8672,#6821,#6822);
#6004=AXIS2_PLACEMENT_3D('',#8673,#6823,#6824);
#6005=AXIS2_PLACEMENT_3D('',#8674,#6825,#6826);
#6006=AXIS2_PLACEMENT_3D('',#8675,#6827,#6828);
#6007=AXIS2_PLACEMENT_3D('',#8676,#6829,#6830);
#6008=AXIS2_PLACEMENT_3D('',#8677,#6831,#6832);
#6009=AXIS2_PLACEMENT_3D('',#8678,#6833,#6834);
#6010=AXIS2_PLACEMENT_3D('',#8680,#6835,#6836);
#6011=AXIS2_PLACEMENT_3D('',#8682,#6838,#6839);
#6012=AXIS2_PLACEMENT_3D('',#8683,#6840,#6841);
#6013=AXIS2_PLACEMENT_3D('',#8684,#6842,#6843);
#6014=AXIS2_PLACEMENT_3D('',#8693,#6848,#6849);
#6015=AXIS2_PLACEMENT_3D('',#8699,#6853,#6854);
#6016=AXIS2_PLACEMENT_3D('',#8705,#6858,#6859);
#6017=AXIS2_PLACEMENT_3D('',#8708,#6862,#6863);
#6018=AXIS2_PLACEMENT_3D('',#8709,#6864,#6865);
#6019=AXIS2_PLACEMENT_3D('',#8710,#6866,#6867);
#6020=AXIS2_PLACEMENT_3D('',#8711,#6868,#6869);
#6021=AXIS2_PLACEMENT_3D('',#8725,#6876,#6877);
#6022=AXIS2_PLACEMENT_3D('',#8726,#6878,#6879);
#6023=AXIS2_PLACEMENT_3D('',#8732,#6883,#6884);
#6024=AXIS2_PLACEMENT_3D('',#8736,#6887,#6888);
#6025=AXIS2_PLACEMENT_3D('',#8740,#6891,#6892);
#6026=AXIS2_PLACEMENT_3D('',#8744,#6895,#6896);
#6027=AXIS2_PLACEMENT_3D('',#8748,#6899,#6900);
#6028=AXIS2_PLACEMENT_3D('',#8750,#6902,#6903);
#6029=AXIS2_PLACEMENT_3D('',#8751,#6904,#6905);
#6030=AXIS2_PLACEMENT_3D('',#8753,#6906,#6907);
#6031=AXIS2_PLACEMENT_3D('',#8755,#6909,#6910);
#6032=AXIS2_PLACEMENT_3D('',#8756,#6911,#6912);
#6033=AXIS2_PLACEMENT_3D('',#8757,#6913,#6914);
#6034=AXIS2_PLACEMENT_3D('',#8759,#6915,#6916);
#6035=AXIS2_PLACEMENT_3D('',#8762,#6918,#6919);
#6036=AXIS2_PLACEMENT_3D('',#8763,#6920,#6921);
#6037=AXIS2_PLACEMENT_3D('',#8765,#6922,#6923);
#6038=AXIS2_PLACEMENT_3D('',#8766,#6924,#6925);
#6039=AXIS2_PLACEMENT_3D('',#8768,#6926,#6927);
#6040=AXIS2_PLACEMENT_3D('',#8770,#6929,#6930);
#6041=AXIS2_PLACEMENT_3D('',#8772,#6931,#6932);
#6042=AXIS2_PLACEMENT_3D('',#8775,#6934,#6935);
#6043=AXIS2_PLACEMENT_3D('',#8776,#6936,#6937);
#6044=AXIS2_PLACEMENT_3D('',#8778,#6938,#6939);
#6045=AXIS2_PLACEMENT_3D('',#8779,#6940,#6941);
#6046=AXIS2_PLACEMENT_3D('',#8781,#6942,#6943);
#6047=AXIS2_PLACEMENT_3D('',#8783,#6945,#6946);
#6048=AXIS2_PLACEMENT_3D('',#8785,#6947,#6948);
#6049=AXIS2_PLACEMENT_3D('',#8788,#6950,#6951);
#6050=AXIS2_PLACEMENT_3D('',#8789,#6952,#6953);
#6051=AXIS2_PLACEMENT_3D('',#8791,#6954,#6955);
#6052=AXIS2_PLACEMENT_3D('',#8792,#6956,#6957);
#6053=AXIS2_PLACEMENT_3D('',#8795,#6959,#6960);
#6054=AXIS2_PLACEMENT_3D('',#8796,#6961,#6962);
#6055=AXIS2_PLACEMENT_3D('',#8805,#6967,#6968);
#6056=AXIS2_PLACEMENT_3D('',#8811,#6972,#6973);
#6057=AXIS2_PLACEMENT_3D('',#8817,#6977,#6978);
#6058=AXIS2_PLACEMENT_3D('',#8820,#6981,#6982);
#6059=AXIS2_PLACEMENT_3D('',#8821,#6983,#6984);
#6060=AXIS2_PLACEMENT_3D('',#8822,#6985,#6986);
#6061=AXIS2_PLACEMENT_3D('',#8823,#6987,#6988);
#6062=AXIS2_PLACEMENT_3D('',#8825,#6989,#6990);
#6063=AXIS2_PLACEMENT_3D('',#8828,#6992,#6993);
#6064=AXIS2_PLACEMENT_3D('',#8829,#6994,#6995);
#6065=AXIS2_PLACEMENT_3D('',#8831,#6996,#6997);
#6066=AXIS2_PLACEMENT_3D('',#8832,#6998,#6999);
#6067=AXIS2_PLACEMENT_3D('',#8834,#7000,#7001);
#6068=AXIS2_PLACEMENT_3D('',#8836,#7003,#7004);
#6069=AXIS2_PLACEMENT_3D('',#8838,#7005,#7006);
#6070=AXIS2_PLACEMENT_3D('',#8841,#7008,#7009);
#6071=AXIS2_PLACEMENT_3D('',#8842,#7010,#7011);
#6072=AXIS2_PLACEMENT_3D('',#8844,#7012,#7013);
#6073=AXIS2_PLACEMENT_3D('',#8845,#7014,#7015);
#6074=AXIS2_PLACEMENT_3D('',#8847,#7016,#7017);
#6075=AXIS2_PLACEMENT_3D('',#8849,#7019,#7020);
#6076=AXIS2_PLACEMENT_3D('',#8851,#7021,#7022);
#6077=AXIS2_PLACEMENT_3D('',#8854,#7024,#7025);
#6078=AXIS2_PLACEMENT_3D('',#8855,#7026,#7027);
#6079=AXIS2_PLACEMENT_3D('',#8857,#7028,#7029);
#6080=AXIS2_PLACEMENT_3D('',#8858,#7030,#7031);
#6081=AXIS2_PLACEMENT_3D('',#8861,#7033,#7034);
#6082=AXIS2_PLACEMENT_3D('',#8862,#7035,#7036);
#6083=AXIS2_PLACEMENT_3D('',#8871,#7041,#7042);
#6084=AXIS2_PLACEMENT_3D('',#8877,#7046,#7047);
#6085=AXIS2_PLACEMENT_3D('',#8883,#7051,#7052);
#6086=AXIS2_PLACEMENT_3D('',#8886,#7055,#7056);
#6087=AXIS2_PLACEMENT_3D('',#8887,#7057,#7058);
#6088=AXIS2_PLACEMENT_3D('',#8888,#7059,#7060);
#6089=AXIS2_PLACEMENT_3D('',#8889,#7061,#7062);
#6090=AXIS2_PLACEMENT_3D('',#8891,#7063,#7064);
#6091=AXIS2_PLACEMENT_3D('',#8894,#7066,#7067);
#6092=AXIS2_PLACEMENT_3D('',#8895,#7068,#7069);
#6093=AXIS2_PLACEMENT_3D('',#8897,#7070,#7071);
#6094=AXIS2_PLACEMENT_3D('',#8899,#7073,#7074);
#6095=AXIS2_PLACEMENT_3D('',#8900,#7075,#7076);
#6096=AXIS2_PLACEMENT_3D('',#8902,#7077,#7078);
#6097=AXIS2_PLACEMENT_3D('',#8928,#7080,#7081);
#6098=AXIS2_PLACEMENT_3D('',#8934,#7085,#7086);
#6099=AXIS2_PLACEMENT_3D('',#8938,#7089,#7090);
#6100=AXIS2_PLACEMENT_3D('',#8942,#7093,#7094);
#6101=AXIS2_PLACEMENT_3D('',#8946,#7097,#7098);
#6102=AXIS2_PLACEMENT_3D('',#8950,#7101,#7102);
#6103=AXIS2_PLACEMENT_3D('',#8952,#7104,#7105);
#6104=AXIS2_PLACEMENT_3D('',#8953,#7106,#7107);
#6105=AXIS2_PLACEMENT_3D('',#8954,#7108,#7109);
#6106=AXIS2_PLACEMENT_3D('',#8955,#7110,#7111);
#6107=AXIS2_PLACEMENT_3D('',#8956,#7112,#7113);
#6108=AXIS2_PLACEMENT_3D('',#8958,#7114,#7115);
#6109=AXIS2_PLACEMENT_3D('',#8961,#7117,#7118);
#6110=AXIS2_PLACEMENT_3D('',#8962,#7119,#7120);
#6111=AXIS2_PLACEMENT_3D('',#8963,#7121,#7122);
#6112=AXIS2_PLACEMENT_3D('',#8965,#7123,#7124);
#6113=AXIS2_PLACEMENT_3D('',#8968,#7126,#7127);
#6114=AXIS2_PLACEMENT_3D('',#8969,#7128,#7129);
#6115=AXIS2_PLACEMENT_3D('',#8970,#7130,#7131);
#6116=AXIS2_PLACEMENT_3D('',#8972,#7132,#7133);
#6117=AXIS2_PLACEMENT_3D('',#8975,#7135,#7136);
#6118=AXIS2_PLACEMENT_3D('',#8976,#7137,#7138);
#6119=AXIS2_PLACEMENT_3D('',#8978,#7139,#7140);
#6120=AXIS2_PLACEMENT_3D('',#8981,#7142,#7143);
#6121=AXIS2_PLACEMENT_3D('',#8982,#7144,#7145);
#6122=AXIS2_PLACEMENT_3D('',#8984,#7146,#7147);
#6123=AXIS2_PLACEMENT_3D('',#8987,#7149,#7150);
#6124=AXIS2_PLACEMENT_3D('',#8988,#7151,#7152);
#6125=AXIS2_PLACEMENT_3D('',#8990,#7153,#7154);
#6126=AXIS2_PLACEMENT_3D('',#8993,#7156,#7157);
#6127=AXIS2_PLACEMENT_3D('',#8994,#7158,#7159);
#6128=AXIS2_PLACEMENT_3D('',#8999,#7161,#7162);
#6129=AXIS2_PLACEMENT_3D('',#9002,#7164,#7165);
#6130=AXIS2_PLACEMENT_3D('',#9003,#7166,#7167);
#6131=AXIS2_PLACEMENT_3D('',#9007,#7169,#7170);
#6132=AXIS2_PLACEMENT_3D('',#9009,#7172,#7173);
#6133=AXIS2_PLACEMENT_3D('',#9019,#7179,#7180);
#6134=AXIS2_PLACEMENT_3D('',#9021,#7181,#7182);
#6135=AXIS2_PLACEMENT_3D('',#9024,#7184,#7185);
#6136=AXIS2_PLACEMENT_3D('',#9025,#7186,#7187);
#6137=AXIS2_PLACEMENT_3D('',#9027,#7188,#7189);
#6138=AXIS2_PLACEMENT_3D('',#9030,#7191,#7192);
#6139=AXIS2_PLACEMENT_3D('',#9031,#7193,#7194);
#6140=AXIS2_PLACEMENT_3D('',#9033,#7195,#7196);
#6141=AXIS2_PLACEMENT_3D('',#9034,#7197,#7198);
#6142=AXIS2_PLACEMENT_3D('',#9035,#7199,#7200);
#6143=AXIS2_PLACEMENT_3D('',#9036,#7201,#7202);
#6144=AXIS2_PLACEMENT_3D('',#9037,#7203,#7204);
#6145=AXIS2_PLACEMENT_3D('',#9043,#7208,#7209);
#6146=AXIS2_PLACEMENT_3D('',#9047,#7212,#7213);
#6147=AXIS2_PLACEMENT_3D('',#9051,#7216,#7217);
#6148=AXIS2_PLACEMENT_3D('',#9053,#7219,#7220);
#6149=AXIS2_PLACEMENT_3D('',#9054,#7221,#7222);
#6150=AXIS2_PLACEMENT_3D('',#9055,#7223,#7224);
#6151=AXIS2_PLACEMENT_3D('',#9057,#7225,#7226);
#6152=AXIS2_PLACEMENT_3D('',#9060,#7228,#7229);
#6153=AXIS2_PLACEMENT_3D('',#9061,#7230,#7231);
#6154=AXIS2_PLACEMENT_3D('',#9062,#7232,#7233);
#6155=AXIS2_PLACEMENT_3D('',#9064,#7234,#7235);
#6156=AXIS2_PLACEMENT_3D('',#9067,#7237,#7238);
#6157=AXIS2_PLACEMENT_3D('',#9068,#7239,#7240);
#6158=AXIS2_PLACEMENT_3D('',#9069,#7241,#7242);
#6159=AXIS2_PLACEMENT_3D('',#9071,#7243,#7244);
#6160=AXIS2_PLACEMENT_3D('',#9074,#7246,#7247);
#6161=AXIS2_PLACEMENT_3D('',#9075,#7248,#7249);
#6162=AXIS2_PLACEMENT_3D('',#9077,#7250,#7251);
#6163=AXIS2_PLACEMENT_3D('',#9080,#7253,#7254);
#6164=AXIS2_PLACEMENT_3D('',#9081,#7255,#7256);
#6165=AXIS2_PLACEMENT_3D('',#9083,#7257,#7258);
#6166=AXIS2_PLACEMENT_3D('',#9086,#7260,#7261);
#6167=AXIS2_PLACEMENT_3D('',#9087,#7262,#7263);
#6168=AXIS2_PLACEMENT_3D('',#9089,#7264,#7265);
#6169=AXIS2_PLACEMENT_3D('',#9092,#7267,#7268);
#6170=AXIS2_PLACEMENT_3D('',#9093,#7269,#7270);
#6171=AXIS2_PLACEMENT_3D('',#9098,#7272,#7273);
#6172=AXIS2_PLACEMENT_3D('',#9101,#7275,#7276);
#6173=AXIS2_PLACEMENT_3D('',#9102,#7277,#7278);
#6174=AXIS2_PLACEMENT_3D('',#9106,#7280,#7281);
#6175=AXIS2_PLACEMENT_3D('',#9108,#7283,#7284);
#6176=AXIS2_PLACEMENT_3D('',#9118,#7290,#7291);
#6177=AXIS2_PLACEMENT_3D('',#9120,#7292,#7293);
#6178=AXIS2_PLACEMENT_3D('',#9123,#7295,#7296);
#6179=AXIS2_PLACEMENT_3D('',#9124,#7297,#7298);
#6180=AXIS2_PLACEMENT_3D('',#9126,#7299,#7300);
#6181=AXIS2_PLACEMENT_3D('',#9129,#7302,#7303);
#6182=AXIS2_PLACEMENT_3D('',#9130,#7304,#7305);
#6183=AXIS2_PLACEMENT_3D('',#9131,#7306,#7307);
#6184=AXIS2_PLACEMENT_3D('',#9133,#7308,#7309);
#6185=AXIS2_PLACEMENT_3D('',#9134,#7310,#7311);
#6186=AXIS2_PLACEMENT_3D('',#9135,#7312,#7313);
#6187=AXIS2_PLACEMENT_3D('',#9136,#7314,#7315);
#6188=AXIS2_PLACEMENT_3D('',#9142,#7319,#7320);
#6189=AXIS2_PLACEMENT_3D('',#9146,#7323,#7324);
#6190=AXIS2_PLACEMENT_3D('',#9150,#7327,#7328);
#6191=AXIS2_PLACEMENT_3D('',#9152,#7330,#7331);
#6192=AXIS2_PLACEMENT_3D('',#9153,#7332,#7333);
#6193=AXIS2_PLACEMENT_3D('',#9154,#7334,#7335);
#6194=AXIS2_PLACEMENT_3D('',#9156,#7336,#7337);
#6195=AXIS2_PLACEMENT_3D('',#9159,#7339,#7340);
#6196=AXIS2_PLACEMENT_3D('',#9160,#7341,#7342);
#6197=AXIS2_PLACEMENT_3D('',#9162,#7343,#7344);
#6198=AXIS2_PLACEMENT_3D('',#9165,#7346,#7347);
#6199=AXIS2_PLACEMENT_3D('',#9166,#7348,#7349);
#6200=AXIS2_PLACEMENT_3D('',#9168,#7350,#7351);
#6201=AXIS2_PLACEMENT_3D('',#9171,#7353,#7354);
#6202=AXIS2_PLACEMENT_3D('',#9172,#7355,#7356);
#6203=AXIS2_PLACEMENT_3D('',#9174,#7357,#7358);
#6204=AXIS2_PLACEMENT_3D('',#9177,#7360,#7361);
#6205=AXIS2_PLACEMENT_3D('',#9178,#7362,#7363);
#6206=AXIS2_PLACEMENT_3D('',#9187,#7368,#7369);
#6207=AXIS2_PLACEMENT_3D('',#9196,#7374,#7375);
#6208=AXIS2_PLACEMENT_3D('',#9202,#7379,#7380);
#6209=AXIS2_PLACEMENT_3D('',#9208,#7384,#7385);
#6210=AXIS2_PLACEMENT_3D('',#9209,#7386,#7387);
#6211=AXIS2_PLACEMENT_3D('',#9219,#7393,#7394);
#6212=AXIS2_PLACEMENT_3D('',#9223,#7397,#7398);
#6213=AXIS2_PLACEMENT_3D('',#9227,#7401,#7402);
#6214=AXIS2_PLACEMENT_3D('',#9228,#7403,#7404);
#6215=AXIS2_PLACEMENT_3D('',#9229,#7405,#7406);
#6216=AXIS2_PLACEMENT_3D('',#9233,#7409,#7410);
#6217=AXIS2_PLACEMENT_3D('',#9237,#7413,#7414);
#6218=AXIS2_PLACEMENT_3D('',#9239,#7416,#7417);
#6219=AXIS2_PLACEMENT_3D('',#9240,#7418,#7419);
#6220=AXIS2_PLACEMENT_3D('',#9241,#7420,#7421);
#6221=AXIS2_PLACEMENT_3D('',#9243,#7422,#7423);
#6222=AXIS2_PLACEMENT_3D('',#9245,#7424,#7425);
#6223=AXIS2_PLACEMENT_3D('',#9246,#7426,#7427);
#6224=AXIS2_PLACEMENT_3D('',#9248,#7428,#7429);
#6225=AXIS2_PLACEMENT_3D('',#9250,#7431,#7432);
#6226=AXIS2_PLACEMENT_3D('',#9252,#7433,#7434);
#6227=AXIS2_PLACEMENT_3D('',#9253,#7435,#7436);
#6228=AXIS2_PLACEMENT_3D('',#9256,#7438,#7439);
#6229=AXIS2_PLACEMENT_3D('',#9257,#7440,#7441);
#6230=AXIS2_PLACEMENT_3D('',#9260,#7443,#7444);
#6231=AXIS2_PLACEMENT_3D('',#9261,#7445,#7446);
#6232=AXIS2_PLACEMENT_3D('',#9262,#7447,#7448);
#6233=AXIS2_PLACEMENT_3D('',#9263,#7449,#7450);
#6234=AXIS2_PLACEMENT_3D('',#9265,#7451,#7452);
#6235=AXIS2_PLACEMENT_3D('',#9266,#7453,#7454);
#6236=AXIS2_PLACEMENT_3D('',#9267,#7455,#7456);
#6237=AXIS2_PLACEMENT_3D('',#9268,#7457,#7458);
#6238=AXIS2_PLACEMENT_3D('',#9270,#7459,#7460);
#6239=AXIS2_PLACEMENT_3D('',#9273,#7462,#7463);
#6240=AXIS2_PLACEMENT_3D('',#9274,#7464,#7465);
#6241=AXIS2_PLACEMENT_3D('',#9276,#7466,#7467);
#6242=AXIS2_PLACEMENT_3D('',#9277,#7468,#7469);
#6243=AXIS2_PLACEMENT_3D('',#9279,#7470,#7471);
#6244=AXIS2_PLACEMENT_3D('',#9281,#7473,#7474);
#6245=AXIS2_PLACEMENT_3D('',#9283,#7475,#7476);
#6246=AXIS2_PLACEMENT_3D('',#9286,#7478,#7479);
#6247=AXIS2_PLACEMENT_3D('',#9287,#7480,#7481);
#6248=AXIS2_PLACEMENT_3D('',#9288,#7482,#7483);
#6249=AXIS2_PLACEMENT_3D('',#9289,#7484,#7485);
#6250=AXIS2_PLACEMENT_3D('',#9290,#7486,#7487);
#6251=AXIS2_PLACEMENT_3D('',#9292,#7488,#7489);
#6252=AXIS2_PLACEMENT_3D('',#9295,#7491,#7492);
#6253=AXIS2_PLACEMENT_3D('',#9296,#7493,#7494);
#6254=AXIS2_PLACEMENT_3D('',#9297,#7495,#7496);
#6255=AXIS2_PLACEMENT_3D('',#9299,#7497,#7498);
#6256=AXIS2_PLACEMENT_3D('',#9302,#7500,#7501);
#6257=AXIS2_PLACEMENT_3D('',#9303,#7502,#7503);
#6258=AXIS2_PLACEMENT_3D('',#9304,#7504,#7505);
#6259=AXIS2_PLACEMENT_3D('',#9306,#7506,#7507);
#6260=AXIS2_PLACEMENT_3D('',#9309,#7509,#7510);
#6261=AXIS2_PLACEMENT_3D('',#9310,#7511,#7512);
#6262=AXIS2_PLACEMENT_3D('',#9312,#7513,#7514);
#6263=AXIS2_PLACEMENT_3D('',#9315,#7516,#7517);
#6264=AXIS2_PLACEMENT_3D('',#9316,#7518,#7519);
#6265=AXIS2_PLACEMENT_3D('',#9318,#7520,#7521);
#6266=AXIS2_PLACEMENT_3D('',#9321,#7523,#7524);
#6267=AXIS2_PLACEMENT_3D('',#9322,#7525,#7526);
#6268=AXIS2_PLACEMENT_3D('',#9324,#7527,#7528);
#6269=AXIS2_PLACEMENT_3D('',#9327,#7530,#7531);
#6270=AXIS2_PLACEMENT_3D('',#9328,#7532,#7533);
#6271=AXIS2_PLACEMENT_3D('',#9330,#7534,#7535);
#6272=AXIS2_PLACEMENT_3D('',#9333,#7537,#7538);
#6273=AXIS2_PLACEMENT_3D('',#9334,#7539,#7540);
#6274=AXIS2_PLACEMENT_3D('',#9343,#7545,#7546);
#6275=AXIS2_PLACEMENT_3D('',#9349,#7550,#7551);
#6276=AXIS2_PLACEMENT_3D('',#9355,#7555,#7556);
#6277=AXIS2_PLACEMENT_3D('',#9358,#7559,#7560);
#6278=AXIS2_PLACEMENT_3D('',#9359,#7561,#7562);
#6279=AXIS2_PLACEMENT_3D('',#9360,#7563,#7564);
#6280=AXIS2_PLACEMENT_3D('',#9361,#7565,#7566);
#6281=AXIS2_PLACEMENT_3D('',#9363,#7567,#7568);
#6282=AXIS2_PLACEMENT_3D('',#9365,#7569,#7570);
#6283=AXIS2_PLACEMENT_3D('',#9366,#7571,#7572);
#6284=AXIS2_PLACEMENT_3D('',#9369,#7574,#7575);
#6285=AXIS2_PLACEMENT_3D('',#9370,#7576,#7577);
#6286=AXIS2_PLACEMENT_3D('',#9372,#7578,#7579);
#6287=AXIS2_PLACEMENT_3D('',#9375,#7581,#7582);
#6288=AXIS2_PLACEMENT_3D('',#9376,#7583,#7584);
#6289=AXIS2_PLACEMENT_3D('',#9377,#7585,#7586);
#6290=AXIS2_PLACEMENT_3D('',#9378,#7587,#7588);
#6291=AXIS2_PLACEMENT_3D('',#9379,#7589,#7590);
#6292=AXIS2_PLACEMENT_3D('',#9388,#7595,#7596);
#6293=AXIS2_PLACEMENT_3D('',#9394,#7600,#7601);
#6294=AXIS2_PLACEMENT_3D('',#9400,#7605,#7606);
#6295=AXIS2_PLACEMENT_3D('',#9406,#7610,#7611);
#6296=AXIS2_PLACEMENT_3D('',#9412,#7615,#7616);
#6297=AXIS2_PLACEMENT_3D('',#9415,#7619,#7620);
#6298=AXIS2_PLACEMENT_3D('',#9416,#7621,#7622);
#6299=AXIS2_PLACEMENT_3D('',#9417,#7623,#7624);
#6300=AXIS2_PLACEMENT_3D('',#9419,#7625,#7626);
#6301=AXIS2_PLACEMENT_3D('',#9421,#7627,#7628);
#6302=AXIS2_PLACEMENT_3D('',#9422,#7629,#7630);
#6303=AXIS2_PLACEMENT_3D('',#9425,#7632,#7633);
#6304=AXIS2_PLACEMENT_3D('',#9426,#7634,#7635);
#6305=AXIS2_PLACEMENT_3D('',#9427,#7636,#7637);
#6306=AXIS2_PLACEMENT_3D('',#9429,#7638,#7639);
#6307=AXIS2_PLACEMENT_3D('',#9430,#7640,#7641);
#6308=AXIS2_PLACEMENT_3D('',#9432,#7642,#7643);
#6309=AXIS2_PLACEMENT_3D('',#9434,#7645,#7646);
#6310=AXIS2_PLACEMENT_3D('',#9436,#7647,#7648);
#6311=AXIS2_PLACEMENT_3D('',#9438,#7650,#7651);
#6312=AXIS2_PLACEMENT_3D('',#9440,#7652,#7653);
#6313=AXIS2_PLACEMENT_3D('',#9442,#7655,#7656);
#6314=AXIS2_PLACEMENT_3D('',#9444,#7657,#7658);
#6315=AXIS2_PLACEMENT_3D('',#9445,#7659,#7660);
#6316=AXIS2_PLACEMENT_3D('',#9447,#7661,#7662);
#6317=AXIS2_PLACEMENT_3D('',#9449,#7664,#7665);
#6318=AXIS2_PLACEMENT_3D('',#9451,#7667,#7668);
#6319=AXIS2_PLACEMENT_3D('',#9452,#7669,#7670);
#6320=AXIS2_PLACEMENT_3D('',#9454,#7671,#7672);
#6321=AXIS2_PLACEMENT_3D('',#9457,#7674,#7675);
#6322=AXIS2_PLACEMENT_3D('',#9458,#7676,#7677);
#6323=AXIS2_PLACEMENT_3D('',#9461,#7679,#7680);
#6324=AXIS2_PLACEMENT_3D('',#9462,#7681,#7682);
#6325=AXIS2_PLACEMENT_3D('',#9464,#7683,#7684);
#6326=AXIS2_PLACEMENT_3D('',#9465,#7685,#7686);
#6327=AXIS2_PLACEMENT_3D('',#9468,#7688,#7689);
#6328=AXIS2_PLACEMENT_3D('',#9469,#7690,#7691);
#6329=AXIS2_PLACEMENT_3D('',#9470,#7692,#7693);
#6330=AXIS2_PLACEMENT_3D('',#9471,#7694,#7695);
#6331=AXIS2_PLACEMENT_3D('',#9483,#7697,#7698);
#6332=AXIS2_PLACEMENT_3D('',#9499,#7699,#7700);
#6333=AXIS2_PLACEMENT_3D('',#9501,#7701,#7702);
#6334=AXIS2_PLACEMENT_3D('',#9527,#7704,#7705);
#6335=AXIS2_PLACEMENT_3D('',#9530,#7708,#7709);
#6336=AXIS2_PLACEMENT_3D('',#9532,#7711,#7712);
#6337=AXIS2_PLACEMENT_3D('',#9534,#7714,#7715);
#6338=AXIS2_PLACEMENT_3D('',#9536,#7716,#7717);
#6339=AXIS2_PLACEMENT_3D('',#9539,#7719,#7720);
#6340=AXIS2_PLACEMENT_3D('',#9540,#7721,#7722);
#6341=AXIS2_PLACEMENT_3D('',#9542,#7724,#7725);
#6342=AXIS2_PLACEMENT_3D('',#9544,#7727,#7728);
#6343=AXIS2_PLACEMENT_3D('',#9545,#7729,#7730);
#6344=AXIS2_PLACEMENT_3D('',#9546,#7731,#7732);
#6345=AXIS2_PLACEMENT_3D('',#9547,#7733,#7734);
#6346=AXIS2_PLACEMENT_3D('',#9548,#7735,#7736);
#6347=AXIS2_PLACEMENT_3D('',#9562,#7743,#7744);
#6348=AXIS2_PLACEMENT_3D('',#9563,#7745,#7746);
#6349=AXIS2_PLACEMENT_3D('',#9577,#7753,#7754);
#6350=AXIS2_PLACEMENT_3D('',#9578,#7755,#7756);
#6351=AXIS2_PLACEMENT_3D('',#9581,#7759,#7760);
#6352=AXIS2_PLACEMENT_3D('',#9583,#7762,#7763);
#6353=AXIS2_PLACEMENT_3D('',#9585,#7765,#7766);
#6354=AXIS2_PLACEMENT_3D('',#9587,#7768,#7769);
#6355=AXIS2_PLACEMENT_3D('',#9589,#7771,#7772);
#6356=AXIS2_PLACEMENT_3D('',#9590,#7773,#7774);
#6357=AXIS2_PLACEMENT_3D('',#9593,#7776,#7777);
#6358=AXIS2_PLACEMENT_3D('',#9594,#7778,#7779);
#6359=AXIS2_PLACEMENT_3D('',#9596,#7780,#7781);
#6360=AXIS2_PLACEMENT_3D('',#9598,#7782,#7783);
#6361=AXIS2_PLACEMENT_3D('',#9599,#7784,#7785);
#6362=AXIS2_PLACEMENT_3D('',#9601,#7787,#7788);
#6363=AXIS2_PLACEMENT_3D('',#9603,#7789,#7790);
#6364=AXIS2_PLACEMENT_3D('',#9605,#7792,#7793);
#6365=AXIS2_PLACEMENT_3D('',#9607,#7794,#7795);
#6366=AXIS2_PLACEMENT_3D('',#9609,#7797,#7798);
#6367=AXIS2_PLACEMENT_3D('',#9611,#7799,#7800);
#6368=AXIS2_PLACEMENT_3D('',#9612,#7801,#7802);
#6369=AXIS2_PLACEMENT_3D('',#9614,#7804,#7805);
#6370=AXIS2_PLACEMENT_3D('',#9615,#7806,#7807);
#6371=AXIS2_PLACEMENT_3D('',#9617,#7808,#7809);
#6372=AXIS2_PLACEMENT_3D('',#9620,#7811,#7812);
#6373=AXIS2_PLACEMENT_3D('',#9621,#7813,#7814);
#6374=AXIS2_PLACEMENT_3D('',#9623,#7815,#7816);
#6375=AXIS2_PLACEMENT_3D('',#9626,#7818,#7819);
#6376=AXIS2_PLACEMENT_3D('',#9627,#7820,#7821);
#6377=AXIS2_PLACEMENT_3D('',#9628,#7822,#7823);
#6378=AXIS2_PLACEMENT_3D('',#9629,#7824,#7825);
#6379=AXIS2_PLACEMENT_3D('',#9630,#7826,#7827);
#6380=AXIS2_PLACEMENT_3D('',#9632,#7828,#7829);
#6381=AXIS2_PLACEMENT_3D('',#9633,#7830,#7831);
#6382=AXIS2_PLACEMENT_3D('',#9635,#7832,#7833);
#6383=AXIS2_PLACEMENT_3D('',#9637,#7835,#7836);
#6384=AXIS2_PLACEMENT_3D('',#9639,#7837,#7838);
#6385=AXIS2_PLACEMENT_3D('',#9641,#7840,#7841);
#6386=AXIS2_PLACEMENT_3D('',#9643,#7842,#7843);
#6387=AXIS2_PLACEMENT_3D('',#9645,#7845,#7846);
#6388=AXIS2_PLACEMENT_3D('',#9647,#7847,#7848);
#6389=AXIS2_PLACEMENT_3D('',#9648,#7849,#7850);
#6390=AXIS2_PLACEMENT_3D('',#9650,#7851,#7852);
#6391=AXIS2_PLACEMENT_3D('',#9652,#7854,#7855);
#6392=AXIS2_PLACEMENT_3D('',#9654,#7856,#7857);
#6393=AXIS2_PLACEMENT_3D('',#9656,#7859,#7860);
#6394=AXIS2_PLACEMENT_3D('',#9658,#7861,#7862);
#6395=AXIS2_PLACEMENT_3D('',#9660,#7864,#7865);
#6396=AXIS2_PLACEMENT_3D('',#9661,#7866,#7867);
#6397=AXIS2_PLACEMENT_3D('',#9670,#7872,#7873);
#6398=AXIS2_PLACEMENT_3D('',#9676,#7877,#7878);
#6399=AXIS2_PLACEMENT_3D('',#9682,#7882,#7883);
#6400=AXIS2_PLACEMENT_3D('',#9688,#7887,#7888);
#6401=AXIS2_PLACEMENT_3D('',#9694,#7892,#7893);
#6402=AXIS2_PLACEMENT_3D('',#9697,#7896,#7897);
#6403=AXIS2_PLACEMENT_3D('',#9698,#7898,#7899);
#6404=AXIS2_PLACEMENT_3D('',#9699,#7900,#7901);
#6405=AXIS2_PLACEMENT_3D('',#9700,#7902,#7903);
#6406=AXIS2_PLACEMENT_3D('',#9702,#7904,#7905);
#6407=AXIS2_PLACEMENT_3D('',#9705,#7907,#7908);
#6408=AXIS2_PLACEMENT_3D('',#9706,#7909,#7910);
#6409=AXIS2_PLACEMENT_3D('',#9707,#7911,#7912);
#6410=AXIS2_PLACEMENT_3D('',#9708,#7913,#7914);
#6411=AXIS2_PLACEMENT_3D('',#9709,#7915,#7916);
#6412=AXIS2_PLACEMENT_3D('',#9710,#7917,#7918);
#6413=AXIS2_PLACEMENT_3D('',#9713,#7919,#7920);
#6414=AXIS2_PLACEMENT_3D('',#9719,#7924,#7925);
#6415=AXIS2_PLACEMENT_3D('',#9721,#7926,#7927);
#6416=AXIS2_PLACEMENT_3D('',#9726,#7930,#7931);
#6417=AXIS2_PLACEMENT_3D('',#9727,#7932,#7933);
#6418=AXIS2_PLACEMENT_3D('',#9729,#7934,#7935);
#6419=AXIS2_PLACEMENT_3D('',#9733,#7938,#7939);
#6420=AXIS2_PLACEMENT_3D('',#9734,#7940,#7941);
#6421=AXIS2_PLACEMENT_3D('',#9736,#7943,#7944);
#6422=AXIS2_PLACEMENT_3D('',#9737,#7945,#7946);
#6423=AXIS2_PLACEMENT_3D('',#9739,#7947,#7948);
#6424=AXIS2_PLACEMENT_3D('',#9742,#7950,#7951);
#6425=AXIS2_PLACEMENT_3D('',#9743,#7952,#7953);
#6426=AXIS2_PLACEMENT_3D('',#9745,#7954,#7955);
#6427=AXIS2_PLACEMENT_3D('',#9746,#7956,#7957);
#6428=AXIS2_PLACEMENT_3D('',#9747,#7958,#7959);
#6429=AXIS2_PLACEMENT_3D('',#9749,#7960,#7961);
#6430=AXIS2_PLACEMENT_3D('',#9752,#7963,#7964);
#6431=AXIS2_PLACEMENT_3D('',#9753,#7965,#7966);
#6432=AXIS2_PLACEMENT_3D('',#9754,#7967,#7968);
#6433=AXIS2_PLACEMENT_3D('',#9757,#7969,#7970);
#6434=AXIS2_PLACEMENT_3D('',#9761,#7973,#7974);
#6435=AXIS2_PLACEMENT_3D('',#9764,#7975,#7976);
#6436=AXIS2_PLACEMENT_3D('',#9768,#7979,#7980);
#6437=AXIS2_PLACEMENT_3D('',#9771,#7981,#7982);
#6438=AXIS2_PLACEMENT_3D('',#9775,#7985,#7986);
#6439=AXIS2_PLACEMENT_3D('',#9778,#7987,#7988);
#6440=AXIS2_PLACEMENT_3D('',#9782,#7991,#7992);
#6441=AXIS2_PLACEMENT_3D('',#9789,#7997,#7998);
#6442=AXIS2_PLACEMENT_3D('',#9794,#8002,#8003);
#6443=AXIS2_PLACEMENT_3D('',#9799,#8007,#8008);
#6444=AXIS2_PLACEMENT_3D('',#9802,#8011,#8012);
#6445=AXIS2_PLACEMENT_3D('',#9803,#8013,#8014);
#6446=AXIS2_PLACEMENT_3D('',#9804,#8015,#8016);
#6447=AXIS2_PLACEMENT_3D('',#9805,#8017,#8018);
#6448=AXIS2_PLACEMENT_3D('',#9807,#8019,#8020);
#6449=AXIS2_PLACEMENT_3D('',#9808,#8021,#8022);
#6450=AXIS2_PLACEMENT_3D('',#9809,#8023,#8024);
#6451=AXIS2_PLACEMENT_3D('',#9810,#8025,#8026);
#6452=AXIS2_PLACEMENT_3D('',#9811,#8027,#8028);
#6453=AXIS2_PLACEMENT_3D('',#9812,#8029,#8030);
#6454=AXIS2_PLACEMENT_3D('',#9813,#8031,#8032);
#6455=AXIS2_PLACEMENT_3D('',#9822,#8037,#8038);
#6456=AXIS2_PLACEMENT_3D('',#9828,#8042,#8043);
#6457=AXIS2_PLACEMENT_3D('',#9834,#8047,#8048);
#6458=AXIS2_PLACEMENT_3D('',#9837,#8051,#8052);
#6459=AXIS2_PLACEMENT_3D('',#9838,#8053,#8054);
#6460=AXIS2_PLACEMENT_3D('',#9841,#8056,#8057);
#6461=AXIS2_PLACEMENT_3D('',#9842,#8058,#8059);
#6462=AXIS2_PLACEMENT_3D('',#9843,#8060,#8061);
#6463=AXIS2_PLACEMENT_3D('',#9844,#8062,#8063);
#6464=AXIS2_PLACEMENT_3D('',#9853,#8068,#8069);
#6465=AXIS2_PLACEMENT_3D('',#9859,#8073,#8074);
#6466=AXIS2_PLACEMENT_3D('',#9865,#8078,#8079);
#6467=AXIS2_PLACEMENT_3D('',#9868,#8082,#8083);
#6468=AXIS2_PLACEMENT_3D('',#9877,#8088,#8089);
#6469=AXIS2_PLACEMENT_3D('',#9883,#8093,#8094);
#6470=AXIS2_PLACEMENT_3D('',#9889,#8098,#8099);
#6471=AXIS2_PLACEMENT_3D('',#9892,#8102,#8103);
#6472=AXIS2_PLACEMENT_3D('',#9893,#8104,#8105);
#6473=AXIS2_PLACEMENT_3D('',#9894,#8106,#8107);
#6474=AXIS2_PLACEMENT_3D('',#9895,#8108,#8109);
#6475=AXIS2_PLACEMENT_3D('',#9897,#8110,#8111);
#6476=AXIS2_PLACEMENT_3D('',#9900,#8113,#8114);
#6477=AXIS2_PLACEMENT_3D('',#9901,#8115,#8116);
#6478=AXIS2_PLACEMENT_3D('',#9903,#8117,#8118);
#6479=AXIS2_PLACEMENT_3D('',#9906,#8120,#8121);
#6480=AXIS2_PLACEMENT_3D('',#9907,#8122,#8123);
#6481=AXIS2_PLACEMENT_3D('',#9908,#8124,#8125);
#6482=AXIS2_PLACEMENT_3D('',#9909,#8126,#8127);
#6483=AXIS2_PLACEMENT_3D('',#9910,#8128,#8129);
#6484=AXIS2_PLACEMENT_3D('',#9919,#8134,#8135);
#6485=AXIS2_PLACEMENT_3D('',#9925,#8139,#8140);
#6486=AXIS2_PLACEMENT_3D('',#9931,#8144,#8145);
#6487=AXIS2_PLACEMENT_3D('',#9934,#8148,#8149);
#6488=AXIS2_PLACEMENT_3D('',#9935,#8150,#8151);
#6489=AXIS2_PLACEMENT_3D('',#9936,#8152,#8153);
#6490=AXIS2_PLACEMENT_3D('',#9937,#8154,#8155);
#6491=AXIS2_PLACEMENT_3D('',#9946,#8160,#8161);
#6492=AXIS2_PLACEMENT_3D('',#9952,#8165,#8166);
#6493=AXIS2_PLACEMENT_3D('',#9958,#8170,#8171);
#6494=AXIS2_PLACEMENT_3D('',#9964,#8175,#8176);
#6495=AXIS2_PLACEMENT_3D('',#9970,#8180,#8181);
#6496=AXIS2_PLACEMENT_3D('',#9973,#8184,#8185);
#6497=AXIS2_PLACEMENT_3D('',#9974,#8186,#8187);
#6498=AXIS2_PLACEMENT_3D('',#9975,#8188,#8189);
#6499=AXIS2_PLACEMENT_3D('',#9977,#8190,#8191);
#6500=AXIS2_PLACEMENT_3D('',#9978,#8192,#8193);
#6501=AXIS2_PLACEMENT_3D('',#9980,#8194,#8195);
#6502=AXIS2_PLACEMENT_3D('',#9981,#8196,#8197);
#6503=AXIS2_PLACEMENT_3D('',#9983,#8198,#8199);
#6504=AXIS2_PLACEMENT_3D('',#9985,#8201,#8202);
#6505=AXIS2_PLACEMENT_3D('',#9987,#8203,#8204);
#6506=AXIS2_PLACEMENT_3D('',#9989,#8206,#8207);
#6507=AXIS2_PLACEMENT_3D('',#9991,#8208,#8209);
#6508=AXIS2_PLACEMENT_3D('',#9993,#8211,#8212);
#6509=AXIS2_PLACEMENT_3D('',#9995,#8213,#8214);
#6510=AXIS2_PLACEMENT_3D('',#9996,#8215,#8216);
#6511=AXIS2_PLACEMENT_3D('',#9998,#8217,#8218);
#6512=AXIS2_PLACEMENT_3D('',#10000,#8220,#8221);
#6513=AXIS2_PLACEMENT_3D('',#10002,#8223,#8224);
#6514=AXIS2_PLACEMENT_3D('',#10003,#8225,#8226);
#6515=AXIS2_PLACEMENT_3D('',#10004,#8227,#8228);
#6516=AXIS2_PLACEMENT_3D('',#10005,#8229,#8230);
#6517=AXIS2_PLACEMENT_3D('',#10006,#8231,#8232);
#6518=AXIS2_PLACEMENT_3D('',#10007,#8233,#8234);
#6519=AXIS2_PLACEMENT_3D('',#10008,#8235,#8236);
#6520=AXIS2_PLACEMENT_3D('',#10009,#8237,#8238);
#6521=AXIS2_PLACEMENT_3D('',#10010,#8239,#8240);
#6522=AXIS2_PLACEMENT_3D('',#10011,#8241,#8242);
#6523=AXIS2_PLACEMENT_3D('',#10012,#8243,#8244);
#6524=AXIS2_PLACEMENT_3D('',#10013,#8245,#8246);
#6525=AXIS2_PLACEMENT_3D('',#10014,#8247,#8248);
#6526=AXIS2_PLACEMENT_3D('',#10015,#8249,#8250);
#6527=AXIS2_PLACEMENT_3D('',#10016,#8251,#8252);
#6528=AXIS2_PLACEMENT_3D('',#10017,#8253,#8254);
#6529=AXIS2_PLACEMENT_3D('',#10018,#8255,#8256);
#6530=AXIS2_PLACEMENT_3D('',#10019,#8257,#8258);
#6531=AXIS2_PLACEMENT_3D('',#10020,#8259,#8260);
#6532=AXIS2_PLACEMENT_3D('',#10021,#8261,#8262);
#6533=AXIS2_PLACEMENT_3D('',#10022,#8263,#8264);
#6534=AXIS2_PLACEMENT_3D('',#10023,#8265,#8266);
#6535=AXIS2_PLACEMENT_3D('',#10024,#8267,#8268);
#6536=AXIS2_PLACEMENT_3D('',#10025,#8269,#8270);
#6537=AXIS2_PLACEMENT_3D('',#10026,#8271,#8272);
#6538=AXIS2_PLACEMENT_3D('',#10027,#8273,#8274);
#6539=AXIS2_PLACEMENT_3D('',#10028,#8275,#8276);
#6540=AXIS2_PLACEMENT_3D('',#10029,#8277,#8278);
#6541=AXIS2_PLACEMENT_3D('',#10030,#8279,#8280);
#6542=AXIS2_PLACEMENT_3D('',#10031,#8281,#8282);
#6543=AXIS2_PLACEMENT_3D('',#10032,#8283,#8284);
#6544=AXIS2_PLACEMENT_3D('',#10033,#8285,#8286);
#6545=AXIS2_PLACEMENT_3D('',#10034,#8287,#8288);
#6546=AXIS2_PLACEMENT_3D('',#10035,#8289,#8290);
#6547=AXIS2_PLACEMENT_3D('',#10036,#8291,#8292);
#6548=AXIS2_PLACEMENT_3D('',#10037,#8293,#8294);
#6549=AXIS2_PLACEMENT_3D('',#10038,#8295,#8296);
#6550=AXIS2_PLACEMENT_3D('',#10039,#8297,#8298);
#6551=AXIS2_PLACEMENT_3D('',#10040,#8299,#8300);
#6552=AXIS2_PLACEMENT_3D('',#10041,#8301,#8302);
#6553=AXIS2_PLACEMENT_3D('',#10042,#8303,#8304);
#6554=AXIS2_PLACEMENT_3D('',#10043,#8305,#8306);
#6555=AXIS2_PLACEMENT_3D('',#10044,#8307,#8308);
#6556=AXIS2_PLACEMENT_3D('',#10045,#8309,#8310);
#6557=AXIS2_PLACEMENT_3D('',#10046,#8311,#8312);
#6558=AXIS2_PLACEMENT_3D('',#10047,#8313,#8314);
#6559=AXIS2_PLACEMENT_3D('',#10048,#8315,#8316);
#6560=AXIS2_PLACEMENT_3D('',#10049,#8317,#8318);
#6561=AXIS2_PLACEMENT_3D('',#10050,#8319,#8320);
#6562=AXIS2_PLACEMENT_3D('',#10051,#8321,#8322);
#6563=AXIS2_PLACEMENT_3D('',#10052,#8323,#8324);
#6564=AXIS2_PLACEMENT_3D('',#10053,#8325,#8326);
#6565=AXIS2_PLACEMENT_3D('',#10054,#8327,#8328);
#6566=AXIS2_PLACEMENT_3D('',#10055,#8329,#8330);
#6567=AXIS2_PLACEMENT_3D('',#10056,#8331,#8332);
#6568=AXIS2_PLACEMENT_3D('',#10057,#8333,#8334);
#6569=DIRECTION('axis',(0.,0.,1.));
#6570=DIRECTION('refdir',(1.,0.,0.));
#6571=DIRECTION('axis',(0.,0.,1.));
#6572=DIRECTION('refdir',(1.,0.,0.));
#6573=DIRECTION('axis',(0.,0.,1.));
#6574=DIRECTION('refdir',(1.,0.,0.));
#6575=DIRECTION('center_axis',(0.,0.,1.));
#6576=DIRECTION('ref_axis',(1.,0.,0.));
#6577=DIRECTION('center_axis',(0.,0.,1.));
#6578=DIRECTION('ref_axis',(1.,0.,0.));
#6579=DIRECTION('',(0.,0.,1.));
#6580=DIRECTION('center_axis',(0.,0.,1.));
#6581=DIRECTION('ref_axis',(1.,0.,0.));
#6582=DIRECTION('center_axis',(0.,0.,1.));
#6583=DIRECTION('ref_axis',(1.,0.,0.));
#6584=DIRECTION('center_axis',(0.,0.,1.));
#6585=DIRECTION('ref_axis',(1.,0.,0.));
#6586=DIRECTION('center_axis',(0.,0.,1.));
#6587=DIRECTION('ref_axis',(1.,0.,0.));
#6588=DIRECTION('',(0.,0.,1.));
#6589=DIRECTION('center_axis',(0.,0.,1.));
#6590=DIRECTION('ref_axis',(1.,0.,0.));
#6591=DIRECTION('center_axis',(0.,0.,1.));
#6592=DIRECTION('ref_axis',(1.,0.,0.));
#6593=DIRECTION('center_axis',(1.,0.,0.));
#6594=DIRECTION('ref_axis',(0.,0.,-1.));
#6595=DIRECTION('center_axis',(1.,0.,0.));
#6596=DIRECTION('ref_axis',(0.,0.,-1.));
#6597=DIRECTION('',(1.,0.,0.));
#6598=DIRECTION('center_axis',(-1.,0.,0.));
#6599=DIRECTION('ref_axis',(0.,0.,-1.));
#6600=DIRECTION('center_axis',(1.,0.,0.));
#6601=DIRECTION('ref_axis',(0.,0.,-1.));
#6602=DIRECTION('center_axis',(1.,0.,0.));
#6603=DIRECTION('ref_axis',(0.,0.,-1.));
#6604=DIRECTION('center_axis',(1.,0.,0.));
#6605=DIRECTION('ref_axis',(0.,0.,-1.));
#6606=DIRECTION('center_axis',(1.,0.,0.));
#6607=DIRECTION('ref_axis',(0.,0.,-1.));
#6608=DIRECTION('',(1.,0.,0.));
#6609=DIRECTION('center_axis',(1.,0.,0.));
#6610=DIRECTION('ref_axis',(0.,0.,-1.));
#6611=DIRECTION('center_axis',(1.,0.,0.));
#6612=DIRECTION('ref_axis',(0.,0.,-1.));
#6613=DIRECTION('center_axis',(-1.,0.,0.));
#6614=DIRECTION('ref_axis',(0.,0.,-1.));
#6615=DIRECTION('center_axis',(0.,1.,0.));
#6616=DIRECTION('ref_axis',(1.,0.,0.));
#6617=DIRECTION('',(1.,0.,0.));
#6618=DIRECTION('center_axis',(0.,1.,0.));
#6619=DIRECTION('ref_axis',(1.,0.,0.));
#6620=DIRECTION('center_axis',(0.,1.,0.));
#6621=DIRECTION('ref_axis',(1.,0.,0.));
#6622=DIRECTION('center_axis',(-0.707106781186548,0.707106781186548,0.));
#6623=DIRECTION('ref_axis',(0.707106781186547,0.707106781186547,0.));
#6624=DIRECTION('center_axis',(0.707106781186548,0.707106781186547,0.));
#6625=DIRECTION('ref_axis',(0.707106781186547,-0.707106781186548,0.));
#6626=DIRECTION('center_axis',(0.,1.,0.));
#6627=DIRECTION('ref_axis',(1.,0.,0.));
#6628=DIRECTION('center_axis',(0.707106781186548,0.707106781186547,0.));
#6629=DIRECTION('ref_axis',(0.707106781186547,-0.707106781186548,0.));
#6630=DIRECTION('center_axis',(0.,1.,0.));
#6631=DIRECTION('ref_axis',(1.,0.,0.));
#6632=DIRECTION('center_axis',(-0.707106781186548,0.707106781186548,0.));
#6633=DIRECTION('ref_axis',(0.707106781186547,0.707106781186547,0.));
#6634=DIRECTION('center_axis',(0.,1.,0.));
#6635=DIRECTION('ref_axis',(1.,0.,0.));
#6636=DIRECTION('center_axis',(-0.707106781186548,-0.707106781186547,0.));
#6637=DIRECTION('ref_axis',(0.707106781186547,-0.707106781186548,0.));
#6638=DIRECTION('center_axis',(0.707106781186548,-0.707106781186548,0.));
#6639=DIRECTION('ref_axis',(0.707106781186547,0.707106781186547,0.));
#6640=DIRECTION('center_axis',(0.,1.,0.));
#6641=DIRECTION('ref_axis',(1.,0.,0.));
#6642=DIRECTION('center_axis',(0.,1.,0.));
#6643=DIRECTION('ref_axis',(1.,0.,0.));
#6644=DIRECTION('center_axis',(0.707106781186548,-0.707106781186548,0.));
#6645=DIRECTION('ref_axis',(0.707106781186547,0.707106781186547,0.));
#6646=DIRECTION('center_axis',(-0.707106781186548,-0.707106781186547,0.));
#6647=DIRECTION('ref_axis',(0.707106781186547,-0.707106781186548,0.));
#6648=DIRECTION('center_axis',(0.,1.,0.));
#6649=DIRECTION('ref_axis',(1.,0.,0.));
#6650=DIRECTION('center_axis',(0.,1.,0.));
#6651=DIRECTION('ref_axis',(1.,0.,0.));
#6652=DIRECTION('',(-1.,0.,0.));
#6653=DIRECTION('center_axis',(1.,0.,0.));
#6654=DIRECTION('ref_axis',(0.,0.,-1.));
#6655=DIRECTION('',(1.,0.,0.));
#6656=DIRECTION('center_axis',(0.707106781186547,-0.707106781186548,0.));
#6657=DIRECTION('ref_axis',(0.707106781186548,0.707106781186547,0.));
#6658=DIRECTION('',(-1.,0.,0.));
#6659=DIRECTION('',(1.,0.,0.));
#6660=DIRECTION('center_axis',(0.707106781186547,-0.707106781186548,0.));
#6661=DIRECTION('ref_axis',(0.707106781186548,0.707106781186547,0.));
#6662=DIRECTION('center_axis',(0.707106781186548,0.707106781186548,0.));
#6663=DIRECTION('ref_axis',(0.707106781186547,-0.707106781186547,0.));
#6664=DIRECTION('',(1.,0.,0.));
#6665=DIRECTION('center_axis',(-0.707106781186547,0.707106781186548,0.));
#6666=DIRECTION('ref_axis',(0.707106781186548,0.707106781186547,0.));
#6667=DIRECTION('center_axis',(-0.707106781186548,-0.707106781186548,0.));
#6668=DIRECTION('ref_axis',(0.707106781186547,-0.707106781186547,0.));
#6669=DIRECTION('',(1.,0.,0.));
#6670=DIRECTION('',(-1.,0.,0.));
#6671=DIRECTION('center_axis',(-0.707106781186548,-0.707106781186548,0.));
#6672=DIRECTION('ref_axis',(0.707106781186547,-0.707106781186547,0.));
#6673=DIRECTION('',(1.,0.,0.));
#6674=DIRECTION('center_axis',(0.707106781186548,-0.707106781186548,0.));
#6675=DIRECTION('ref_axis',(0.707106781186547,0.707106781186547,0.));
#6676=DIRECTION('',(-1.,0.,0.));
#6677=DIRECTION('',(1.,0.,0.));
#6678=DIRECTION('center_axis',(0.707106781186548,-0.707106781186548,0.));
#6679=DIRECTION('ref_axis',(0.707106781186547,0.707106781186547,0.));
#6680=DIRECTION('center_axis',(0.707106781186548,0.707106781186547,0.));
#6681=DIRECTION('ref_axis',(0.707106781186547,-0.707106781186548,0.));
#6682=DIRECTION('',(1.,0.,0.));
#6683=DIRECTION('center_axis',(-0.707106781186548,0.707106781186548,0.));
#6684=DIRECTION('ref_axis',(0.707106781186547,0.707106781186547,0.));
#6685=DIRECTION('center_axis',(-0.707106781186548,-0.707106781186547,0.));
#6686=DIRECTION('ref_axis',(0.707106781186547,-0.707106781186548,0.));
#6687=DIRECTION('',(1.,0.,0.));
#6688=DIRECTION('',(-1.,0.,0.));
#6689=DIRECTION('center_axis',(-0.707106781186548,-0.707106781186547,0.));
#6690=DIRECTION('ref_axis',(0.707106781186547,-0.707106781186548,0.));
#6691=DIRECTION('',(1.,0.,0.));
#6692=DIRECTION('center_axis',(0.707106781186548,-0.707106781186548,0.));
#6693=DIRECTION('ref_axis',(0.707106781186547,0.707106781186547,0.));
#6694=DIRECTION('',(-1.,0.,0.));
#6695=DIRECTION('',(1.,0.,0.));
#6696=DIRECTION('center_axis',(0.707106781186548,-0.707106781186548,0.));
#6697=DIRECTION('ref_axis',(0.707106781186547,0.707106781186547,0.));
#6698=DIRECTION('center_axis',(0.707106781186548,0.707106781186547,0.));
#6699=DIRECTION('ref_axis',(0.707106781186547,-0.707106781186548,0.));
#6700=DIRECTION('',(1.,0.,0.));
#6701=DIRECTION('center_axis',(-0.707106781186548,0.707106781186548,0.));
#6702=DIRECTION('ref_axis',(0.707106781186547,0.707106781186547,0.));
#6703=DIRECTION('center_axis',(-0.707106781186548,-0.707106781186547,0.));
#6704=DIRECTION('ref_axis',(0.707106781186547,-0.707106781186548,0.));
#6705=DIRECTION('',(1.,0.,0.));
#6706=DIRECTION('',(-1.,0.,0.));
#6707=DIRECTION('center_axis',(-0.707106781186548,-0.707106781186547,0.));
#6708=DIRECTION('ref_axis',(0.707106781186547,-0.707106781186548,0.));
#6709=DIRECTION('',(1.,0.,0.));
#6710=DIRECTION('',(-1.,0.,0.));
#6711=DIRECTION('',(1.,0.,0.));
#6712=DIRECTION('',(1.,0.,0.));
#6713=DIRECTION('',(-1.,0.,0.));
#6714=DIRECTION('',(1.,0.,0.));
#6715=DIRECTION('center_axis',(-0.707106781186548,0.707106781186548,0.));
#6716=DIRECTION('ref_axis',(0.707106781186547,0.707106781186547,0.));
#6717=DIRECTION('',(-1.,0.,0.));
#6718=DIRECTION('center_axis',(0.707106781186548,0.707106781186547,0.));
#6719=DIRECTION('ref_axis',(0.707106781186547,-0.707106781186548,0.));
#6720=DIRECTION('center_axis',(-0.707106781186548,0.707106781186548,0.));
#6721=DIRECTION('ref_axis',(0.707106781186547,0.707106781186547,0.));
#6722=DIRECTION('',(-1.,0.,0.));
#6723=DIRECTION('center_axis',(0.707106781186548,0.707106781186547,0.));
#6724=DIRECTION('ref_axis',(0.707106781186547,-0.707106781186548,0.));
#6725=DIRECTION('center_axis',(-0.707106781186547,0.707106781186548,0.));
#6726=DIRECTION('ref_axis',(0.707106781186548,0.707106781186547,0.));
#6727=DIRECTION('',(-1.,0.,0.));
#6728=DIRECTION('center_axis',(0.707106781186548,0.707106781186548,0.));
#6729=DIRECTION('ref_axis',(0.707106781186547,-0.707106781186547,0.));
#6730=DIRECTION('center_axis',(0.,1.,0.));
#6731=DIRECTION('ref_axis',(1.,0.,0.));
#6732=DIRECTION('center_axis',(0.,1.,0.));
#6733=DIRECTION('ref_axis',(1.,0.,0.));
#6734=DIRECTION('center_axis',(0.,1.,0.));
#6735=DIRECTION('ref_axis',(1.,0.,0.));
#6736=DIRECTION('center_axis',(0.,1.,0.));
#6737=DIRECTION('ref_axis',(1.,0.,0.));
#6738=DIRECTION('',(0.,1.,0.));
#6739=DIRECTION('center_axis',(0.,1.,0.));
#6740=DIRECTION('ref_axis',(1.,0.,0.));
#6741=DIRECTION('center_axis',(0.,1.,0.));
#6742=DIRECTION('ref_axis',(1.,0.,0.));
#6743=DIRECTION('center_axis',(0.,1.,0.));
#6744=DIRECTION('ref_axis',(1.,0.,0.));
#6745=DIRECTION('center_axis',(0.,1.,0.));
#6746=DIRECTION('ref_axis',(1.,0.,0.));
#6747=DIRECTION('center_axis',(0.,1.,0.));
#6748=DIRECTION('ref_axis',(1.,0.,0.));
#6749=DIRECTION('center_axis',(0.,1.,0.));
#6750=DIRECTION('ref_axis',(1.,0.,0.));
#6751=DIRECTION('center_axis',(0.,1.,0.));
#6752=DIRECTION('ref_axis',(1.,0.,0.));
#6753=DIRECTION('center_axis',(0.,1.,0.));
#6754=DIRECTION('ref_axis',(1.,0.,0.));
#6755=DIRECTION('center_axis',(0.,1.,0.));
#6756=DIRECTION('ref_axis',(1.,0.,0.));
#6757=DIRECTION('center_axis',(0.,1.,0.));
#6758=DIRECTION('ref_axis',(1.,0.,0.));
#6759=DIRECTION('center_axis',(0.,1.,0.));
#6760=DIRECTION('ref_axis',(1.,0.,0.));
#6761=DIRECTION('center_axis',(0.,1.,0.));
#6762=DIRECTION('ref_axis',(1.,0.,0.));
#6763=DIRECTION('center_axis',(0.,1.,0.));
#6764=DIRECTION('ref_axis',(1.,0.,0.));
#6765=DIRECTION('center_axis',(0.,1.,0.));
#6766=DIRECTION('ref_axis',(1.,0.,0.));
#6767=DIRECTION('center_axis',(0.,1.,0.));
#6768=DIRECTION('ref_axis',(1.,0.,0.));
#6769=DIRECTION('center_axis',(0.,1.,0.));
#6770=DIRECTION('ref_axis',(1.,0.,0.));
#6771=DIRECTION('',(0.,1.,0.));
#6772=DIRECTION('center_axis',(0.,1.,0.));
#6773=DIRECTION('ref_axis',(1.,0.,0.));
#6774=DIRECTION('center_axis',(0.,1.,0.));
#6775=DIRECTION('ref_axis',(1.,0.,0.));
#6776=DIRECTION('center_axis',(0.,1.,0.));
#6777=DIRECTION('ref_axis',(1.,0.,0.));
#6778=DIRECTION('center_axis',(0.,1.,0.));
#6779=DIRECTION('ref_axis',(1.,0.,0.));
#6780=DIRECTION('center_axis',(0.,1.,0.));
#6781=DIRECTION('ref_axis',(1.,0.,0.));
#6782=DIRECTION('center_axis',(0.,1.,0.));
#6783=DIRECTION('ref_axis',(1.,0.,0.));
#6784=DIRECTION('center_axis',(0.,1.,0.));
#6785=DIRECTION('ref_axis',(1.,0.,0.));
#6786=DIRECTION('center_axis',(0.,1.,0.));
#6787=DIRECTION('ref_axis',(1.,0.,0.));
#6788=DIRECTION('center_axis',(0.,1.,0.));
#6789=DIRECTION('ref_axis',(1.,0.,0.));
#6790=DIRECTION('center_axis',(0.,1.,0.));
#6791=DIRECTION('ref_axis',(1.,0.,0.));
#6792=DIRECTION('center_axis',(0.,1.,0.));
#6793=DIRECTION('ref_axis',(1.,0.,0.));
#6794=DIRECTION('center_axis',(0.,1.,0.));
#6795=DIRECTION('ref_axis',(1.,0.,0.));
#6796=DIRECTION('center_axis',(0.,1.,0.));
#6797=DIRECTION('ref_axis',(1.,0.,0.));
#6798=DIRECTION('center_axis',(0.,1.,0.));
#6799=DIRECTION('ref_axis',(1.,0.,0.));
#6800=DIRECTION('center_axis',(0.,1.,0.));
#6801=DIRECTION('ref_axis',(1.,0.,0.));
#6802=DIRECTION('center_axis',(0.,1.,0.));
#6803=DIRECTION('ref_axis',(1.,0.,0.));
#6804=DIRECTION('',(0.,1.,0.));
#6805=DIRECTION('center_axis',(0.,1.,0.));
#6806=DIRECTION('ref_axis',(1.,0.,0.));
#6807=DIRECTION('center_axis',(0.,1.,0.));
#6808=DIRECTION('ref_axis',(1.,0.,0.));
#6809=DIRECTION('center_axis',(0.,1.,0.));
#6810=DIRECTION('ref_axis',(1.,0.,0.));
#6811=DIRECTION('center_axis',(0.,1.,0.));
#6812=DIRECTION('ref_axis',(1.,0.,0.));
#6813=DIRECTION('center_axis',(0.,1.,0.));
#6814=DIRECTION('ref_axis',(1.,0.,0.));
#6815=DIRECTION('center_axis',(0.,1.,0.));
#6816=DIRECTION('ref_axis',(1.,0.,0.));
#6817=DIRECTION('center_axis',(0.,1.,0.));
#6818=DIRECTION('ref_axis',(1.,0.,0.));
#6819=DIRECTION('center_axis',(0.,1.,0.));
#6820=DIRECTION('ref_axis',(1.,0.,0.));
#6821=DIRECTION('center_axis',(0.,1.,0.));
#6822=DIRECTION('ref_axis',(1.,0.,0.));
#6823=DIRECTION('center_axis',(0.,1.,0.));
#6824=DIRECTION('ref_axis',(1.,0.,0.));
#6825=DIRECTION('center_axis',(0.,1.,0.));
#6826=DIRECTION('ref_axis',(1.,0.,0.));
#6827=DIRECTION('center_axis',(0.,1.,0.));
#6828=DIRECTION('ref_axis',(1.,0.,0.));
#6829=DIRECTION('center_axis',(0.,1.,0.));
#6830=DIRECTION('ref_axis',(1.,0.,0.));
#6831=DIRECTION('center_axis',(0.,1.,0.));
#6832=DIRECTION('ref_axis',(1.,0.,0.));
#6833=DIRECTION('center_axis',(0.,1.,0.));
#6834=DIRECTION('ref_axis',(1.,0.,0.));
#6835=DIRECTION('center_axis',(0.,1.,0.));
#6836=DIRECTION('ref_axis',(1.,0.,0.));
#6837=DIRECTION('',(0.,1.,0.));
#6838=DIRECTION('center_axis',(0.,1.,0.));
#6839=DIRECTION('ref_axis',(1.,0.,0.));
#6840=DIRECTION('center_axis',(0.,1.,0.));
#6841=DIRECTION('ref_axis',(1.,0.,0.));
#6842=DIRECTION('center_axis',(0.,1.,0.));
#6843=DIRECTION('ref_axis',(-1.,0.,0.));
#6844=DIRECTION('',(-1.,0.,0.));
#6845=DIRECTION('',(0.,0.,1.));
#6846=DIRECTION('',(-1.,0.,0.));
#6847=DIRECTION('',(0.,0.,1.));
#6848=DIRECTION('center_axis',(1.,0.,0.));
#6849=DIRECTION('ref_axis',(0.,1.,0.));
#6850=DIRECTION('',(0.,1.,0.));
#6851=DIRECTION('',(0.,1.,0.));
#6852=DIRECTION('',(0.,0.,1.));
#6853=DIRECTION('center_axis',(0.,-1.,0.));
#6854=DIRECTION('ref_axis',(1.,0.,0.));
#6855=DIRECTION('',(1.,0.,0.));
#6856=DIRECTION('',(1.,0.,0.));
#6857=DIRECTION('',(0.,0.,1.));
#6858=DIRECTION('center_axis',(-1.,0.,0.));
#6859=DIRECTION('ref_axis',(0.,-1.,0.));
#6860=DIRECTION('',(0.,-1.,0.));
#6861=DIRECTION('',(0.,-1.,0.));
#6862=DIRECTION('center_axis',(0.,0.,1.));
#6863=DIRECTION('ref_axis',(1.,0.,0.));
#6864=DIRECTION('center_axis',(0.,0.,1.));
#6865=DIRECTION('ref_axis',(1.,0.,0.));
#6866=DIRECTION('axis',(0.,0.,1.));
#6867=DIRECTION('refdir',(1.,0.,0.));
#6868=DIRECTION('center_axis',(1.,0.,0.));
#6869=DIRECTION('ref_axis',(0.,0.,-1.));
#6870=DIRECTION('',(0.,0.5,0.866025403784439));
#6871=DIRECTION('',(0.,-0.5,0.866025403784439));
#6872=DIRECTION('',(0.,-1.,0.));
#6873=DIRECTION('',(0.,-0.500000000000001,-0.866025403784438));
#6874=DIRECTION('',(0.,0.5,-0.866025403784439));
#6875=DIRECTION('',(0.,1.,0.));
#6876=DIRECTION('center_axis',(1.,0.,0.));
#6877=DIRECTION('ref_axis',(0.,0.,-1.));
#6878=DIRECTION('center_axis',(0.,0.,-1.));
#6879=DIRECTION('ref_axis',(0.,1.,0.));
#6880=DIRECTION('',(0.,1.,0.));
#6881=DIRECTION('',(1.,0.,0.));
#6882=DIRECTION('',(1.,0.,0.));
#6883=DIRECTION('center_axis',(0.,-0.866025403784439,-0.5));
#6884=DIRECTION('ref_axis',(0.,0.5,-0.866025403784439));
#6885=DIRECTION('',(0.,0.5,-0.866025403784439));
#6886=DIRECTION('',(1.,0.,0.));
#6887=DIRECTION('center_axis',(0.,-0.866025403784438,0.500000000000001));
#6888=DIRECTION('ref_axis',(0.,-0.500000000000001,-0.866025403784438));
#6889=DIRECTION('',(0.,-0.500000000000001,-0.866025403784438));
#6890=DIRECTION('',(1.,0.,0.));
#6891=DIRECTION('center_axis',(0.,0.,1.));
#6892=DIRECTION('ref_axis',(0.,-1.,0.));
#6893=DIRECTION('',(0.,-1.,0.));
#6894=DIRECTION('',(1.,0.,0.));
#6895=DIRECTION('center_axis',(0.,0.866025403784439,0.5));
#6896=DIRECTION('ref_axis',(0.,-0.5,0.866025403784439));
#6897=DIRECTION('',(0.,-0.5,0.866025403784439));
#6898=DIRECTION('',(1.,0.,0.));
#6899=DIRECTION('center_axis',(0.,0.866025403784439,-0.5));
#6900=DIRECTION('ref_axis',(0.,0.5,0.866025403784439));
#6901=DIRECTION('',(0.,0.5,0.866025403784439));
#6902=DIRECTION('center_axis',(1.,0.,0.));
#6903=DIRECTION('ref_axis',(0.,0.,-1.));
#6904=DIRECTION('center_axis',(1.,0.,0.));
#6905=DIRECTION('ref_axis',(0.,0.,-1.));
#6906=DIRECTION('center_axis',(1.,0.,0.));
#6907=DIRECTION('ref_axis',(0.,0.,-1.));
#6908=DIRECTION('',(-1.,0.,0.));
#6909=DIRECTION('center_axis',(1.,0.,0.));
#6910=DIRECTION('ref_axis',(0.,0.,-1.));
#6911=DIRECTION('axis',(0.,0.,1.));
#6912=DIRECTION('refdir',(1.,0.,0.));
#6913=DIRECTION('center_axis',(0.,0.,1.));
#6914=DIRECTION('ref_axis',(1.,0.,0.));
#6915=DIRECTION('center_axis',(0.,0.,1.));
#6916=DIRECTION('ref_axis',(1.,0.,0.));
#6917=DIRECTION('',(0.,0.,1.));
#6918=DIRECTION('center_axis',(0.,0.,-1.));
#6919=DIRECTION('ref_axis',(1.,0.,0.));
#6920=DIRECTION('center_axis',(0.,0.,1.));
#6921=DIRECTION('ref_axis',(1.,0.,0.));
#6922=DIRECTION('center_axis',(0.,0.,1.));
#6923=DIRECTION('ref_axis',(1.,0.,0.));
#6924=DIRECTION('center_axis',(0.,0.,1.));
#6925=DIRECTION('ref_axis',(1.,0.,0.));
#6926=DIRECTION('center_axis',(0.,0.,1.));
#6927=DIRECTION('ref_axis',(1.,0.,0.));
#6928=DIRECTION('',(0.,0.,1.));
#6929=DIRECTION('center_axis',(0.,0.,1.));
#6930=DIRECTION('ref_axis',(1.,0.,0.));
#6931=DIRECTION('center_axis',(0.,0.,1.));
#6932=DIRECTION('ref_axis',(1.,0.,0.));
#6933=DIRECTION('',(0.,0.,1.));
#6934=DIRECTION('center_axis',(0.,0.,-1.));
#6935=DIRECTION('ref_axis',(1.,0.,0.));
#6936=DIRECTION('center_axis',(0.,0.,1.));
#6937=DIRECTION('ref_axis',(1.,0.,0.));
#6938=DIRECTION('center_axis',(0.,0.,1.));
#6939=DIRECTION('ref_axis',(1.,0.,0.));
#6940=DIRECTION('center_axis',(0.,0.,1.));
#6941=DIRECTION('ref_axis',(1.,0.,0.));
#6942=DIRECTION('center_axis',(0.,0.,1.));
#6943=DIRECTION('ref_axis',(1.,0.,0.));
#6944=DIRECTION('',(0.,0.,1.));
#6945=DIRECTION('center_axis',(0.,0.,1.));
#6946=DIRECTION('ref_axis',(1.,0.,0.));
#6947=DIRECTION('center_axis',(0.,0.,1.));
#6948=DIRECTION('ref_axis',(1.,0.,0.));
#6949=DIRECTION('',(0.,0.,1.));
#6950=DIRECTION('center_axis',(0.,0.,1.));
#6951=DIRECTION('ref_axis',(1.,0.,0.));
#6952=DIRECTION('center_axis',(0.,0.,1.));
#6953=DIRECTION('ref_axis',(1.,0.,0.));
#6954=DIRECTION('center_axis',(0.,0.,-1.));
#6955=DIRECTION('ref_axis',(1.,0.,0.));
#6956=DIRECTION('center_axis',(0.,0.,1.));
#6957=DIRECTION('ref_axis',(1.,0.,0.));
#6958=DIRECTION('',(0.,0.,1.));
#6959=DIRECTION('center_axis',(0.,0.,-1.));
#6960=DIRECTION('ref_axis',(1.,0.,0.));
#6961=DIRECTION('center_axis',(0.,1.,0.));
#6962=DIRECTION('ref_axis',(-1.,0.,0.));
#6963=DIRECTION('',(-1.,0.,0.));
#6964=DIRECTION('',(0.,0.,1.));
#6965=DIRECTION('',(-1.,0.,0.));
#6966=DIRECTION('',(0.,0.,1.));
#6967=DIRECTION('center_axis',(1.,0.,0.));
#6968=DIRECTION('ref_axis',(0.,1.,0.));
#6969=DIRECTION('',(0.,1.,0.));
#6970=DIRECTION('',(0.,1.,0.));
#6971=DIRECTION('',(0.,0.,1.));
#6972=DIRECTION('center_axis',(0.,-1.,0.));
#6973=DIRECTION('ref_axis',(1.,0.,0.));
#6974=DIRECTION('',(1.,0.,0.));
#6975=DIRECTION('',(1.,0.,0.));
#6976=DIRECTION('',(0.,0.,1.));
#6977=DIRECTION('center_axis',(-1.,0.,0.));
#6978=DIRECTION('ref_axis',(0.,-1.,0.));
#6979=DIRECTION('',(0.,-1.,0.));
#6980=DIRECTION('',(0.,-1.,0.));
#6981=DIRECTION('center_axis',(0.,0.,1.));
#6982=DIRECTION('ref_axis',(1.,0.,0.));
#6983=DIRECTION('center_axis',(0.,0.,1.));
#6984=DIRECTION('ref_axis',(1.,0.,0.));
#6985=DIRECTION('axis',(0.,0.,1.));
#6986=DIRECTION('refdir',(1.,0.,0.));
#6987=DIRECTION('center_axis',(0.,0.,1.));
#6988=DIRECTION('ref_axis',(1.,0.,0.));
#6989=DIRECTION('center_axis',(0.,0.,1.));
#6990=DIRECTION('ref_axis',(1.,0.,0.));
#6991=DIRECTION('',(0.,0.,1.));
#6992=DIRECTION('center_axis',(0.,0.,-1.));
#6993=DIRECTION('ref_axis',(1.,0.,0.));
#6994=DIRECTION('center_axis',(0.,0.,1.));
#6995=DIRECTION('ref_axis',(1.,0.,0.));
#6996=DIRECTION('center_axis',(0.,0.,1.));
#6997=DIRECTION('ref_axis',(1.,0.,0.));
#6998=DIRECTION('center_axis',(0.,0.,1.));
#6999=DIRECTION('ref_axis',(1.,0.,0.));
#7000=DIRECTION('center_axis',(0.,0.,1.));
#7001=DIRECTION('ref_axis',(1.,0.,0.));
#7002=DIRECTION('',(0.,0.,1.));
#7003=DIRECTION('center_axis',(0.,0.,1.));
#7004=DIRECTION('ref_axis',(1.,0.,0.));
#7005=DIRECTION('center_axis',(0.,0.,1.));
#7006=DIRECTION('ref_axis',(1.,0.,0.));
#7007=DIRECTION('',(0.,0.,1.));
#7008=DIRECTION('center_axis',(0.,0.,-1.));
#7009=DIRECTION('ref_axis',(1.,0.,0.));
#7010=DIRECTION('center_axis',(0.,0.,1.));
#7011=DIRECTION('ref_axis',(1.,0.,0.));
#7012=DIRECTION('center_axis',(0.,0.,1.));
#7013=DIRECTION('ref_axis',(1.,0.,0.));
#7014=DIRECTION('center_axis',(0.,0.,1.));
#7015=DIRECTION('ref_axis',(1.,0.,0.));
#7016=DIRECTION('center_axis',(0.,0.,1.));
#7017=DIRECTION('ref_axis',(1.,0.,0.));
#7018=DIRECTION('',(0.,0.,1.));
#7019=DIRECTION('center_axis',(0.,0.,1.));
#7020=DIRECTION('ref_axis',(1.,0.,0.));
#7021=DIRECTION('center_axis',(0.,0.,1.));
#7022=DIRECTION('ref_axis',(1.,0.,0.));
#7023=DIRECTION('',(0.,0.,1.));
#7024=DIRECTION('center_axis',(0.,0.,1.));
#7025=DIRECTION('ref_axis',(1.,0.,0.));
#7026=DIRECTION('center_axis',(0.,0.,1.));
#7027=DIRECTION('ref_axis',(1.,0.,0.));
#7028=DIRECTION('center_axis',(0.,0.,-1.));
#7029=DIRECTION('ref_axis',(1.,0.,0.));
#7030=DIRECTION('center_axis',(0.,0.,1.));
#7031=DIRECTION('ref_axis',(1.,0.,0.));
#7032=DIRECTION('',(0.,0.,1.));
#7033=DIRECTION('center_axis',(0.,0.,-1.));
#7034=DIRECTION('ref_axis',(1.,0.,0.));
#7035=DIRECTION('center_axis',(0.,1.,0.));
#7036=DIRECTION('ref_axis',(-1.,0.,0.));
#7037=DIRECTION('',(-1.,0.,0.));
#7038=DIRECTION('',(0.,0.,1.));
#7039=DIRECTION('',(-1.,0.,0.));
#7040=DIRECTION('',(0.,0.,1.));
#7041=DIRECTION('center_axis',(1.,0.,0.));
#7042=DIRECTION('ref_axis',(0.,1.,0.));
#7043=DIRECTION('',(0.,1.,0.));
#7044=DIRECTION('',(0.,1.,0.));
#7045=DIRECTION('',(0.,0.,1.));
#7046=DIRECTION('center_axis',(0.,-1.,0.));
#7047=DIRECTION('ref_axis',(1.,0.,0.));
#7048=DIRECTION('',(1.,0.,0.));
#7049=DIRECTION('',(1.,0.,0.));
#7050=DIRECTION('',(0.,0.,1.));
#7051=DIRECTION('center_axis',(-1.,0.,0.));
#7052=DIRECTION('ref_axis',(0.,-1.,0.));
#7053=DIRECTION('',(0.,-1.,0.));
#7054=DIRECTION('',(0.,-1.,0.));
#7055=DIRECTION('center_axis',(0.,0.,1.));
#7056=DIRECTION('ref_axis',(1.,0.,0.));
#7057=DIRECTION('center_axis',(0.,0.,1.));
#7058=DIRECTION('ref_axis',(1.,0.,0.));
#7059=DIRECTION('axis',(0.,0.,1.));
#7060=DIRECTION('refdir',(1.,0.,0.));
#7061=DIRECTION('center_axis',(0.,-1.,0.));
#7062=DIRECTION('ref_axis',(1.,0.,0.));
#7063=DIRECTION('center_axis',(0.,1.,0.));
#7064=DIRECTION('ref_axis',(1.,0.,0.));
#7065=DIRECTION('',(0.,1.,0.));
#7066=DIRECTION('center_axis',(0.,-1.,0.));
#7067=DIRECTION('ref_axis',(1.,0.,0.));
#7068=DIRECTION('center_axis',(0.,1.,0.));
#7069=DIRECTION('ref_axis',(1.,0.,0.));
#7070=DIRECTION('center_axis',(0.,-1.,0.));
#7071=DIRECTION('ref_axis',(1.,0.,0.));
#7072=DIRECTION('',(-0.707106781186547,0.707106781186548,-8.65956056235493E-17));
#7073=DIRECTION('center_axis',(0.,-1.,0.));
#7074=DIRECTION('ref_axis',(0.,0.,-1.));
#7075=DIRECTION('center_axis',(0.,-1.,0.));
#7076=DIRECTION('ref_axis',(1.,0.,0.));
#7077=DIRECTION('center_axis',(0.,1.,0.));
#7078=DIRECTION('ref_axis',(1.,0.,0.));
#7079=DIRECTION('',(-0.866025403784439,-0.5,-1.06057523872491E-16));
#7080=DIRECTION('center_axis',(1.92296268638356E-16,0.,-1.));
#7081=DIRECTION('ref_axis',(-1.,0.,-1.92296268638356E-16));
#7082=DIRECTION('',(0.,1.,0.));
#7083=DIRECTION('',(-1.,0.,-1.92296268638356E-16));
#7084=DIRECTION('',(0.,1.,0.));
#7085=DIRECTION('center_axis',(0.866025403784439,0.,-0.5));
#7086=DIRECTION('ref_axis',(-0.5,0.,-0.866025403784439));
#7087=DIRECTION('',(0.,1.,0.));
#7088=DIRECTION('',(-0.5,0.,-0.866025403784439));
#7089=DIRECTION('center_axis',(0.866025403784439,0.,0.5));
#7090=DIRECTION('ref_axis',(0.5,0.,-0.866025403784439));
#7091=DIRECTION('',(0.,1.,0.));
#7092=DIRECTION('',(0.5,0.,-0.866025403784439));
#7093=DIRECTION('center_axis',(-1.92296268638356E-16,0.,1.));
#7094=DIRECTION('ref_axis',(1.,0.,1.92296268638356E-16));
#7095=DIRECTION('',(0.,1.,0.));
#7096=DIRECTION('',(1.,0.,1.92296268638356E-16));
#7097=DIRECTION('center_axis',(-0.866025403784439,0.,0.5));
#7098=DIRECTION('ref_axis',(0.5,0.,0.866025403784439));
#7099=DIRECTION('',(0.,1.,0.));
#7100=DIRECTION('',(0.5,0.,0.866025403784439));
#7101=DIRECTION('center_axis',(-0.866025403784439,0.,-0.5));
#7102=DIRECTION('ref_axis',(-0.5,0.,0.866025403784439));
#7103=DIRECTION('',(-0.5,0.,0.866025403784438));
#7104=DIRECTION('center_axis',(0.,1.,0.));
#7105=DIRECTION('ref_axis',(0.,0.,1.));
#7106=DIRECTION('center_axis',(0.,1.,0.));
#7107=DIRECTION('ref_axis',(1.,0.,0.));
#7108=DIRECTION('axis',(0.,0.,1.));
#7109=DIRECTION('refdir',(1.,0.,0.));
#7110=DIRECTION('axis',(0.,0.,1.));
#7111=DIRECTION('refdir',(1.,0.,0.));
#7112=DIRECTION('center_axis',(0.,0.,1.));
#7113=DIRECTION('ref_axis',(1.,0.,0.));
#7114=DIRECTION('center_axis',(0.,0.,1.));
#7115=DIRECTION('ref_axis',(1.,0.,0.));
#7116=DIRECTION('',(0.,0.,1.));
#7117=DIRECTION('center_axis',(0.,0.,-1.));
#7118=DIRECTION('ref_axis',(1.,0.,0.));
#7119=DIRECTION('center_axis',(0.,0.,1.));
#7120=DIRECTION('ref_axis',(1.,0.,0.));
#7121=DIRECTION('center_axis',(0.,0.,1.));
#7122=DIRECTION('ref_axis',(1.,0.,0.));
#7123=DIRECTION('center_axis',(0.,0.,1.));
#7124=DIRECTION('ref_axis',(1.,0.,0.));
#7125=DIRECTION('',(0.,0.,1.));
#7126=DIRECTION('center_axis',(0.,0.,-1.));
#7127=DIRECTION('ref_axis',(1.,0.,0.));
#7128=DIRECTION('center_axis',(0.,0.,1.));
#7129=DIRECTION('ref_axis',(1.,0.,0.));
#7130=DIRECTION('center_axis',(0.,1.,0.));
#7131=DIRECTION('ref_axis',(1.,0.,0.));
#7132=DIRECTION('center_axis',(0.,1.,0.));
#7133=DIRECTION('ref_axis',(1.,0.,0.));
#7134=DIRECTION('',(0.,1.,0.));
#7135=DIRECTION('center_axis',(0.,-1.,0.));
#7136=DIRECTION('ref_axis',(1.,0.,0.));
#7137=DIRECTION('center_axis',(0.,1.,0.));
#7138=DIRECTION('ref_axis',(1.,0.,0.));
#7139=DIRECTION('center_axis',(0.,1.,0.));
#7140=DIRECTION('ref_axis',(1.,0.,0.));
#7141=DIRECTION('',(0.,1.,0.));
#7142=DIRECTION('center_axis',(0.,-1.,0.));
#7143=DIRECTION('ref_axis',(1.,0.,0.));
#7144=DIRECTION('center_axis',(0.,1.,0.));
#7145=DIRECTION('ref_axis',(1.,0.,0.));
#7146=DIRECTION('center_axis',(0.,1.,0.));
#7147=DIRECTION('ref_axis',(1.,0.,0.));
#7148=DIRECTION('',(0.,1.,0.));
#7149=DIRECTION('center_axis',(0.,-1.,0.));
#7150=DIRECTION('ref_axis',(1.,0.,0.));
#7151=DIRECTION('center_axis',(0.,1.,0.));
#7152=DIRECTION('ref_axis',(1.,0.,0.));
#7153=DIRECTION('center_axis',(0.,1.,0.));
#7154=DIRECTION('ref_axis',(1.,0.,0.));
#7155=DIRECTION('',(0.,1.,0.));
#7156=DIRECTION('center_axis',(0.,-1.,0.));
#7157=DIRECTION('ref_axis',(1.,0.,0.));
#7158=DIRECTION('center_axis',(0.,0.,1.));
#7159=DIRECTION('ref_axis',(1.,0.,0.));
#7160=DIRECTION('',(0.,0.,1.));
#7161=DIRECTION('center_axis',(0.,0.,1.));
#7162=DIRECTION('ref_axis',(1.,0.,0.));
#7163=DIRECTION('',(0.,0.,-1.));
#7164=DIRECTION('center_axis',(0.,0.,-1.));
#7165=DIRECTION('ref_axis',(1.,0.,0.));
#7166=DIRECTION('center_axis',(0.,0.,1.));
#7167=DIRECTION('ref_axis',(1.,0.,0.));
#7168=DIRECTION('',(1.,0.,0.));
#7169=DIRECTION('center_axis',(0.,0.,1.));
#7170=DIRECTION('ref_axis',(0.,-1.,0.));
#7171=DIRECTION('',(1.,0.,0.));
#7172=DIRECTION('center_axis',(0.,0.,1.));
#7173=DIRECTION('ref_axis',(1.,0.,0.));
#7174=DIRECTION('',(-1.,0.,0.));
#7175=DIRECTION('',(0.,-1.,0.));
#7176=DIRECTION('',(1.,0.,0.));
#7177=DIRECTION('',(0.,1.,0.));
#7178=DIRECTION('',(-1.,0.,0.));
#7179=DIRECTION('center_axis',(0.,1.,0.));
#7180=DIRECTION('ref_axis',(1.,0.,0.));
#7181=DIRECTION('center_axis',(0.,1.,0.));
#7182=DIRECTION('ref_axis',(1.,0.,0.));
#7183=DIRECTION('',(0.,1.,0.));
#7184=DIRECTION('center_axis',(0.,-1.,0.));
#7185=DIRECTION('ref_axis',(1.,0.,0.));
#7186=DIRECTION('center_axis',(0.,1.,0.));
#7187=DIRECTION('ref_axis',(1.,0.,0.));
#7188=DIRECTION('center_axis',(0.,1.,0.));
#7189=DIRECTION('ref_axis',(1.,0.,0.));
#7190=DIRECTION('',(0.,1.,0.));
#7191=DIRECTION('center_axis',(0.,1.,0.));
#7192=DIRECTION('ref_axis',(1.,0.,0.));
#7193=DIRECTION('center_axis',(0.,1.,0.));
#7194=DIRECTION('ref_axis',(1.,0.,0.));
#7195=DIRECTION('center_axis',(0.,-1.,0.));
#7196=DIRECTION('ref_axis',(0.,0.,-1.));
#7197=DIRECTION('center_axis',(0.,1.,0.));
#7198=DIRECTION('ref_axis',(1.,0.,0.));
#7199=DIRECTION('center_axis',(6.12323399573677E-17,0.,1.));
#7200=DIRECTION('ref_axis',(1.,0.,0.));
#7201=DIRECTION('center_axis',(0.,-1.,0.));
#7202=DIRECTION('ref_axis',(0.,0.,-1.));
#7203=DIRECTION('center_axis',(0.,1.,0.));
#7204=DIRECTION('ref_axis',(-1.,0.,0.));
#7205=DIRECTION('',(0.,0.,1.));
#7206=DIRECTION('',(-1.,0.,0.));
#7207=DIRECTION('',(0.,0.,1.));
#7208=DIRECTION('center_axis',(1.,0.,0.));
#7209=DIRECTION('ref_axis',(0.,1.,0.));
#7210=DIRECTION('',(0.,1.,0.));
#7211=DIRECTION('',(0.,0.,1.));
#7212=DIRECTION('center_axis',(0.,-1.,0.));
#7213=DIRECTION('ref_axis',(1.,0.,0.));
#7214=DIRECTION('',(1.,0.,0.));
#7215=DIRECTION('',(0.,0.,1.));
#7216=DIRECTION('center_axis',(-1.,0.,0.));
#7217=DIRECTION('ref_axis',(0.,-1.,0.));
#7218=DIRECTION('',(0.,-1.,0.));
#7219=DIRECTION('center_axis',(0.,0.,1.));
#7220=DIRECTION('ref_axis',(1.,0.,0.));
#7221=DIRECTION('axis',(0.,0.,1.));
#7222=DIRECTION('refdir',(1.,0.,0.));
#7223=DIRECTION('center_axis',(0.,0.,1.));
#7224=DIRECTION('ref_axis',(1.,0.,0.));
#7225=DIRECTION('center_axis',(0.,0.,1.));
#7226=DIRECTION('ref_axis',(1.,0.,0.));
#7227=DIRECTION('',(0.,0.,1.));
#7228=DIRECTION('center_axis',(0.,0.,-1.));
#7229=DIRECTION('ref_axis',(1.,0.,0.));
#7230=DIRECTION('center_axis',(0.,0.,1.));
#7231=DIRECTION('ref_axis',(1.,0.,0.));
#7232=DIRECTION('center_axis',(0.,0.,1.));
#7233=DIRECTION('ref_axis',(1.,0.,0.));
#7234=DIRECTION('center_axis',(0.,0.,1.));
#7235=DIRECTION('ref_axis',(1.,0.,0.));
#7236=DIRECTION('',(0.,0.,1.));
#7237=DIRECTION('center_axis',(0.,0.,-1.));
#7238=DIRECTION('ref_axis',(1.,0.,0.));
#7239=DIRECTION('center_axis',(0.,0.,1.));
#7240=DIRECTION('ref_axis',(1.,0.,0.));
#7241=DIRECTION('center_axis',(0.,1.,0.));
#7242=DIRECTION('ref_axis',(1.,0.,0.));
#7243=DIRECTION('center_axis',(0.,1.,0.));
#7244=DIRECTION('ref_axis',(1.,0.,0.));
#7245=DIRECTION('',(0.,1.,0.));
#7246=DIRECTION('center_axis',(0.,-1.,0.));
#7247=DIRECTION('ref_axis',(1.,0.,0.));
#7248=DIRECTION('center_axis',(0.,1.,0.));
#7249=DIRECTION('ref_axis',(1.,0.,0.));
#7250=DIRECTION('center_axis',(0.,1.,0.));
#7251=DIRECTION('ref_axis',(1.,0.,0.));
#7252=DIRECTION('',(0.,1.,0.));
#7253=DIRECTION('center_axis',(0.,-1.,0.));
#7254=DIRECTION('ref_axis',(1.,0.,0.));
#7255=DIRECTION('center_axis',(0.,1.,0.));
#7256=DIRECTION('ref_axis',(1.,0.,0.));
#7257=DIRECTION('center_axis',(0.,1.,0.));
#7258=DIRECTION('ref_axis',(1.,0.,0.));
#7259=DIRECTION('',(0.,1.,0.));
#7260=DIRECTION('center_axis',(0.,-1.,0.));
#7261=DIRECTION('ref_axis',(1.,0.,0.));
#7262=DIRECTION('center_axis',(0.,1.,0.));
#7263=DIRECTION('ref_axis',(1.,0.,0.));
#7264=DIRECTION('center_axis',(0.,1.,0.));
#7265=DIRECTION('ref_axis',(1.,0.,0.));
#7266=DIRECTION('',(0.,1.,0.));
#7267=DIRECTION('center_axis',(0.,-1.,0.));
#7268=DIRECTION('ref_axis',(1.,0.,0.));
#7269=DIRECTION('center_axis',(0.,0.,1.));
#7270=DIRECTION('ref_axis',(1.,0.,0.));
#7271=DIRECTION('',(0.,0.,1.));
#7272=DIRECTION('center_axis',(0.,0.,1.));
#7273=DIRECTION('ref_axis',(1.,0.,0.));
#7274=DIRECTION('',(0.,0.,-1.));
#7275=DIRECTION('center_axis',(0.,0.,-1.));
#7276=DIRECTION('ref_axis',(1.,0.,0.));
#7277=DIRECTION('center_axis',(0.,0.,1.));
#7278=DIRECTION('ref_axis',(1.,0.,0.));
#7279=DIRECTION('',(-1.,0.,0.));
#7280=DIRECTION('center_axis',(0.,0.,1.));
#7281=DIRECTION('ref_axis',(0.,-1.,0.));
#7282=DIRECTION('',(-1.,0.,0.));
#7283=DIRECTION('center_axis',(0.,0.,1.));
#7284=DIRECTION('ref_axis',(1.,0.,0.));
#7285=DIRECTION('',(1.,0.,0.));
#7286=DIRECTION('',(0.,1.,0.));
#7287=DIRECTION('',(-1.,0.,0.));
#7288=DIRECTION('',(0.,-1.,0.));
#7289=DIRECTION('',(1.,0.,0.));
#7290=DIRECTION('center_axis',(0.,1.,0.));
#7291=DIRECTION('ref_axis',(1.,0.,0.));
#7292=DIRECTION('center_axis',(0.,1.,0.));
#7293=DIRECTION('ref_axis',(1.,0.,0.));
#7294=DIRECTION('',(0.,1.,0.));
#7295=DIRECTION('center_axis',(0.,-1.,0.));
#7296=DIRECTION('ref_axis',(1.,0.,0.));
#7297=DIRECTION('center_axis',(0.,1.,0.));
#7298=DIRECTION('ref_axis',(1.,0.,0.));
#7299=DIRECTION('center_axis',(0.,1.,0.));
#7300=DIRECTION('ref_axis',(1.,0.,0.));
#7301=DIRECTION('',(0.,1.,0.));
#7302=DIRECTION('center_axis',(0.,1.,0.));
#7303=DIRECTION('ref_axis',(1.,0.,0.));
#7304=DIRECTION('center_axis',(0.,1.,0.));
#7305=DIRECTION('ref_axis',(1.,0.,0.));
#7306=DIRECTION('center_axis',(0.,1.,0.));
#7307=DIRECTION('ref_axis',(1.,0.,0.));
#7308=DIRECTION('center_axis',(0.,1.,0.));
#7309=DIRECTION('ref_axis',(0.,0.,1.));
#7310=DIRECTION('center_axis',(6.12323399573677E-17,0.,1.));
#7311=DIRECTION('ref_axis',(1.,0.,0.));
#7312=DIRECTION('center_axis',(0.,1.,0.));
#7313=DIRECTION('ref_axis',(0.,0.,1.));
#7314=DIRECTION('center_axis',(0.,1.,0.));
#7315=DIRECTION('ref_axis',(-1.,0.,0.));
#7316=DIRECTION('',(-1.,0.,0.));
#7317=DIRECTION('',(0.,0.,1.));
#7318=DIRECTION('',(0.,0.,1.));
#7319=DIRECTION('center_axis',(1.,0.,0.));
#7320=DIRECTION('ref_axis',(0.,1.,0.));
#7321=DIRECTION('',(0.,1.,0.));
#7322=DIRECTION('',(0.,0.,1.));
#7323=DIRECTION('center_axis',(0.,-1.,0.));
#7324=DIRECTION('ref_axis',(1.,0.,0.));
#7325=DIRECTION('',(0.,0.,1.));
#7326=DIRECTION('',(1.,0.,0.));
#7327=DIRECTION('center_axis',(-1.,0.,0.));
#7328=DIRECTION('ref_axis',(0.,-1.,0.));
#7329=DIRECTION('',(0.,-1.,0.));
#7330=DIRECTION('center_axis',(0.,0.,1.));
#7331=DIRECTION('ref_axis',(1.,0.,0.));
#7332=DIRECTION('axis',(0.,0.,1.));
#7333=DIRECTION('refdir',(1.,0.,0.));
#7334=DIRECTION('center_axis',(0.,1.,0.));
#7335=DIRECTION('ref_axis',(1.,0.,0.));
#7336=DIRECTION('center_axis',(0.,1.,0.));
#7337=DIRECTION('ref_axis',(1.,0.,0.));
#7338=DIRECTION('',(0.,1.,0.));
#7339=DIRECTION('center_axis',(0.,-1.,0.));
#7340=DIRECTION('ref_axis',(1.,0.,0.));
#7341=DIRECTION('center_axis',(0.,1.,0.));
#7342=DIRECTION('ref_axis',(1.,0.,0.));
#7343=DIRECTION('center_axis',(0.,1.,0.));
#7344=DIRECTION('ref_axis',(1.,0.,0.));
#7345=DIRECTION('',(0.,1.,0.));
#7346=DIRECTION('center_axis',(0.,-1.,0.));
#7347=DIRECTION('ref_axis',(1.,0.,0.));
#7348=DIRECTION('center_axis',(0.,1.,0.));
#7349=DIRECTION('ref_axis',(1.,0.,0.));
#7350=DIRECTION('center_axis',(0.,1.,0.));
#7351=DIRECTION('ref_axis',(1.,0.,0.));
#7352=DIRECTION('',(0.,1.,0.));
#7353=DIRECTION('center_axis',(0.,-1.,0.));
#7354=DIRECTION('ref_axis',(1.,0.,0.));
#7355=DIRECTION('center_axis',(0.,1.,0.));
#7356=DIRECTION('ref_axis',(1.,0.,0.));
#7357=DIRECTION('center_axis',(0.,1.,0.));
#7358=DIRECTION('ref_axis',(1.,0.,0.));
#7359=DIRECTION('',(0.,1.,0.));
#7360=DIRECTION('center_axis',(0.,-1.,0.));
#7361=DIRECTION('ref_axis',(1.,0.,0.));
#7362=DIRECTION('center_axis',(-1.,0.,0.));
#7363=DIRECTION('ref_axis',(0.,0.,1.));
#7364=DIRECTION('',(0.,0.,1.));
#7365=DIRECTION('',(0.,1.,0.));
#7366=DIRECTION('',(0.,0.,-1.));
#7367=DIRECTION('',(0.,1.,0.));
#7368=DIRECTION('center_axis',(0.,0.,-1.));
#7369=DIRECTION('ref_axis',(-1.,0.,0.));
#7370=DIRECTION('',(-1.,0.,0.));
#7371=DIRECTION('',(0.,1.,0.));
#7372=DIRECTION('',(1.,0.,0.));
#7373=DIRECTION('',(0.,1.,0.));
#7374=DIRECTION('center_axis',(0.,0.,-1.));
#7375=DIRECTION('ref_axis',(-1.,0.,0.));
#7376=DIRECTION('',(-1.,0.,0.));
#7377=DIRECTION('',(0.,-1.,0.));
#7378=DIRECTION('',(1.,0.,0.));
#7379=DIRECTION('center_axis',(1.,0.,0.));
#7380=DIRECTION('ref_axis',(0.,0.,-1.));
#7381=DIRECTION('',(0.,0.,-1.));
#7382=DIRECTION('',(0.,-1.,0.));
#7383=DIRECTION('',(0.,0.,1.));
#7384=DIRECTION('center_axis',(0.,1.,0.));
#7385=DIRECTION('ref_axis',(0.,0.,1.));
#7386=DIRECTION('center_axis',(0.,-1.,0.));
#7387=DIRECTION('ref_axis',(1.,0.,0.));
#7388=DIRECTION('',(1.,0.,0.));
#7389=DIRECTION('',(0.,0.,-1.));
#7390=DIRECTION('',(-1.,0.,0.));
#7391=DIRECTION('',(0.,0.,1.));
#7392=DIRECTION('',(1.,0.,0.));
#7393=DIRECTION('center_axis',(0.,0.,1.));
#7394=DIRECTION('ref_axis',(1.,0.,0.));
#7395=DIRECTION('',(-1.,0.,0.));
#7396=DIRECTION('',(0.,1.,0.));
#7397=DIRECTION('center_axis',(0.,0.,1.));
#7398=DIRECTION('ref_axis',(1.,0.,0.));
#7399=DIRECTION('',(0.,1.,0.));
#7400=DIRECTION('',(-1.,0.,0.));
#7401=DIRECTION('center_axis',(0.,1.,0.));
#7402=DIRECTION('ref_axis',(-1.83697019872103E-16,0.,-1.));
#7403=DIRECTION('center_axis',(0.,1.,0.));
#7404=DIRECTION('ref_axis',(1.,0.,0.));
#7405=DIRECTION('center_axis',(-1.,0.,0.));
#7406=DIRECTION('ref_axis',(0.,0.,1.));
#7407=DIRECTION('',(0.,0.,-1.));
#7408=DIRECTION('',(0.,1.,0.));
#7409=DIRECTION('center_axis',(0.,0.,-1.));
#7410=DIRECTION('ref_axis',(-1.,0.,0.));
#7411=DIRECTION('',(1.,0.,0.));
#7412=DIRECTION('',(0.,1.,0.));
#7413=DIRECTION('center_axis',(1.,0.,0.));
#7414=DIRECTION('ref_axis',(0.,0.,-1.));
#7415=DIRECTION('',(0.,0.,1.));
#7416=DIRECTION('center_axis',(0.,1.,0.));
#7417=DIRECTION('ref_axis',(1.,0.,0.));
#7418=DIRECTION('axis',(0.,0.,1.));
#7419=DIRECTION('refdir',(1.,0.,0.));
#7420=DIRECTION('center_axis',(0.,0.,1.));
#7421=DIRECTION('ref_axis',(1.,0.,0.));
#7422=DIRECTION('center_axis',(0.,0.,1.));
#7423=DIRECTION('ref_axis',(1.,0.,0.));
#7424=DIRECTION('center_axis',(0.,0.,1.));
#7425=DIRECTION('ref_axis',(1.,0.,0.));
#7426=DIRECTION('center_axis',(0.,0.,1.));
#7427=DIRECTION('ref_axis',(1.,0.,0.));
#7428=DIRECTION('center_axis',(0.,0.,1.));
#7429=DIRECTION('ref_axis',(1.,0.,0.));
#7430=DIRECTION('',(0.,0.,-1.));
#7431=DIRECTION('center_axis',(0.,0.,1.));
#7432=DIRECTION('ref_axis',(1.,0.,0.));
#7433=DIRECTION('center_axis',(0.,0.,-1.));
#7434=DIRECTION('ref_axis',(1.,0.,0.));
#7435=DIRECTION('center_axis',(0.,0.,1.));
#7436=DIRECTION('ref_axis',(1.,0.,0.));
#7437=DIRECTION('',(0.,0.,-1.));
#7438=DIRECTION('center_axis',(0.,0.,-1.));
#7439=DIRECTION('ref_axis',(1.,0.,0.));
#7440=DIRECTION('center_axis',(0.,0.,1.));
#7441=DIRECTION('ref_axis',(1.,0.,0.));
#7442=DIRECTION('',(0.,0.,-1.));
#7443=DIRECTION('center_axis',(0.,0.,1.));
#7444=DIRECTION('ref_axis',(1.,0.,0.));
#7445=DIRECTION('center_axis',(0.,0.,1.));
#7446=DIRECTION('ref_axis',(1.,0.,0.));
#7447=DIRECTION('axis',(0.,0.,1.));
#7448=DIRECTION('refdir',(1.,0.,0.));
#7449=DIRECTION('center_axis',(0.,0.,1.));
#7450=DIRECTION('ref_axis',(1.,0.,0.));
#7451=DIRECTION('center_axis',(1.22464679914735E-16,-1.,0.));
#7452=DIRECTION('ref_axis',(-1.,-1.22464679914735E-16,0.));
#7453=DIRECTION('center_axis',(0.,0.,-1.));
#7454=DIRECTION('ref_axis',(1.,0.,0.));
#7455=DIRECTION('axis',(0.,0.,1.));
#7456=DIRECTION('refdir',(1.,0.,0.));
#7457=DIRECTION('center_axis',(0.,0.,1.));
#7458=DIRECTION('ref_axis',(1.,0.,0.));
#7459=DIRECTION('center_axis',(0.,0.,1.));
#7460=DIRECTION('ref_axis',(1.,0.,0.));
#7461=DIRECTION('',(0.,0.,1.));
#7462=DIRECTION('center_axis',(0.,0.,1.));
#7463=DIRECTION('ref_axis',(1.,0.,0.));
#7464=DIRECTION('center_axis',(0.,0.,1.));
#7465=DIRECTION('ref_axis',(1.,0.,0.));
#7466=DIRECTION('center_axis',(0.,0.,-1.));
#7467=DIRECTION('ref_axis',(1.,0.,0.));
#7468=DIRECTION('center_axis',(0.,0.,1.));
#7469=DIRECTION('ref_axis',(1.,0.,0.));
#7470=DIRECTION('center_axis',(0.,0.,-1.));
#7471=DIRECTION('ref_axis',(1.,0.,0.));
#7472=DIRECTION('',(0.,0.,-1.));
#7473=DIRECTION('center_axis',(0.,0.,1.));
#7474=DIRECTION('ref_axis',(1.,0.,0.));
#7475=DIRECTION('center_axis',(0.,0.,1.));
#7476=DIRECTION('ref_axis',(1.,0.,0.));
#7477=DIRECTION('',(0.,0.,-1.));
#7478=DIRECTION('center_axis',(0.,0.,1.));
#7479=DIRECTION('ref_axis',(1.,0.,0.));
#7480=DIRECTION('center_axis',(0.,0.,1.));
#7481=DIRECTION('ref_axis',(1.,0.,0.));
#7482=DIRECTION('center_axis',(0.,0.,1.));
#7483=DIRECTION('ref_axis',(1.,0.,0.));
#7484=DIRECTION('axis',(0.,0.,1.));
#7485=DIRECTION('refdir',(1.,0.,0.));
#7486=DIRECTION('center_axis',(0.,0.,1.));
#7487=DIRECTION('ref_axis',(1.,0.,0.));
#7488=DIRECTION('center_axis',(0.,0.,1.));
#7489=DIRECTION('ref_axis',(1.,0.,0.));
#7490=DIRECTION('',(0.,0.,1.));
#7491=DIRECTION('center_axis',(0.,0.,-1.));
#7492=DIRECTION('ref_axis',(1.,0.,0.));
#7493=DIRECTION('center_axis',(0.,0.,1.));
#7494=DIRECTION('ref_axis',(1.,0.,0.));
#7495=DIRECTION('center_axis',(0.,0.,1.));
#7496=DIRECTION('ref_axis',(1.,0.,0.));
#7497=DIRECTION('center_axis',(0.,0.,1.));
#7498=DIRECTION('ref_axis',(1.,0.,0.));
#7499=DIRECTION('',(0.,0.,1.));
#7500=DIRECTION('center_axis',(0.,0.,-1.));
#7501=DIRECTION('ref_axis',(1.,0.,0.));
#7502=DIRECTION('center_axis',(0.,0.,1.));
#7503=DIRECTION('ref_axis',(1.,0.,0.));
#7504=DIRECTION('center_axis',(0.,0.,1.));
#7505=DIRECTION('ref_axis',(1.,0.,0.));
#7506=DIRECTION('center_axis',(0.,0.,1.));
#7507=DIRECTION('ref_axis',(1.,0.,0.));
#7508=DIRECTION('',(0.,0.,1.));
#7509=DIRECTION('center_axis',(0.,0.,-1.));
#7510=DIRECTION('ref_axis',(1.,0.,0.));
#7511=DIRECTION('center_axis',(0.,0.,1.));
#7512=DIRECTION('ref_axis',(1.,0.,0.));
#7513=DIRECTION('center_axis',(0.,0.,1.));
#7514=DIRECTION('ref_axis',(1.,0.,0.));
#7515=DIRECTION('',(0.,0.,1.));
#7516=DIRECTION('center_axis',(0.,0.,-1.));
#7517=DIRECTION('ref_axis',(1.,0.,0.));
#7518=DIRECTION('center_axis',(0.,0.,1.));
#7519=DIRECTION('ref_axis',(1.,0.,0.));
#7520=DIRECTION('center_axis',(0.,0.,1.));
#7521=DIRECTION('ref_axis',(1.,0.,0.));
#7522=DIRECTION('',(0.,0.,1.));
#7523=DIRECTION('center_axis',(0.,0.,-1.));
#7524=DIRECTION('ref_axis',(1.,0.,0.));
#7525=DIRECTION('center_axis',(0.,0.,1.));
#7526=DIRECTION('ref_axis',(1.,0.,0.));
#7527=DIRECTION('center_axis',(0.,0.,1.));
#7528=DIRECTION('ref_axis',(1.,0.,0.));
#7529=DIRECTION('',(0.,0.,1.));
#7530=DIRECTION('center_axis',(0.,0.,-1.));
#7531=DIRECTION('ref_axis',(1.,0.,0.));
#7532=DIRECTION('center_axis',(0.,0.,1.));
#7533=DIRECTION('ref_axis',(1.,0.,0.));
#7534=DIRECTION('center_axis',(0.,0.,1.));
#7535=DIRECTION('ref_axis',(1.,0.,0.));
#7536=DIRECTION('',(0.,0.,1.));
#7537=DIRECTION('center_axis',(0.,0.,-1.));
#7538=DIRECTION('ref_axis',(1.,0.,0.));
#7539=DIRECTION('center_axis',(0.,1.,0.));
#7540=DIRECTION('ref_axis',(-1.,0.,0.));
#7541=DIRECTION('',(-1.,0.,0.));
#7542=DIRECTION('',(0.,0.,1.));
#7543=DIRECTION('',(-1.,0.,0.));
#7544=DIRECTION('',(0.,0.,1.));
#7545=DIRECTION('center_axis',(1.,0.,0.));
#7546=DIRECTION('ref_axis',(0.,1.,0.));
#7547=DIRECTION('',(0.,1.,0.));
#7548=DIRECTION('',(0.,1.,0.));
#7549=DIRECTION('',(0.,0.,1.));
#7550=DIRECTION('center_axis',(0.,-1.,0.));
#7551=DIRECTION('ref_axis',(1.,0.,0.));
#7552=DIRECTION('',(1.,0.,0.));
#7553=DIRECTION('',(1.,0.,0.));
#7554=DIRECTION('',(0.,0.,1.));
#7555=DIRECTION('center_axis',(-1.,0.,0.));
#7556=DIRECTION('ref_axis',(0.,-1.,0.));
#7557=DIRECTION('',(0.,-1.,0.));
#7558=DIRECTION('',(0.,-1.,0.));
#7559=DIRECTION('center_axis',(0.,0.,1.));
#7560=DIRECTION('ref_axis',(1.,0.,0.));
#7561=DIRECTION('center_axis',(0.,0.,1.));
#7562=DIRECTION('ref_axis',(1.,0.,0.));
#7563=DIRECTION('axis',(0.,0.,1.));
#7564=DIRECTION('refdir',(1.,0.,0.));
#7565=DIRECTION('center_axis',(6.12323399573677E-17,0.,1.));
#7566=DIRECTION('ref_axis',(1.,0.,0.));
#7567=DIRECTION('center_axis',(0.,-1.,0.));
#7568=DIRECTION('ref_axis',(0.,0.,-1.));
#7569=DIRECTION('center_axis',(0.,1.,0.));
#7570=DIRECTION('ref_axis',(1.,0.,0.));
#7571=DIRECTION('center_axis',(0.,1.,0.));
#7572=DIRECTION('ref_axis',(1.,0.,0.));
#7573=DIRECTION('',(0.,-1.,0.));
#7574=DIRECTION('center_axis',(0.,-1.,0.));
#7575=DIRECTION('ref_axis',(1.,0.,0.));
#7576=DIRECTION('center_axis',(0.,1.,0.));
#7577=DIRECTION('ref_axis',(1.,0.,0.));
#7578=DIRECTION('center_axis',(0.,1.,0.));
#7579=DIRECTION('ref_axis',(1.,0.,0.));
#7580=DIRECTION('',(0.,-1.,0.));
#7581=DIRECTION('center_axis',(0.,1.,0.));
#7582=DIRECTION('ref_axis',(1.,0.,0.));
#7583=DIRECTION('center_axis',(0.,1.,0.));
#7584=DIRECTION('ref_axis',(1.,0.,0.));
#7585=DIRECTION('center_axis',(0.,1.,0.));
#7586=DIRECTION('ref_axis',(1.,0.,0.));
#7587=DIRECTION('axis',(0.,0.,1.));
#7588=DIRECTION('refdir',(1.,0.,0.));
#7589=DIRECTION('center_axis',(0.866025403784439,0.,-0.5));
#7590=DIRECTION('ref_axis',(0.5,0.,0.866025403784439));
#7591=DIRECTION('',(-0.5,0.,-0.866025403784439));
#7592=DIRECTION('',(0.,-1.,0.));
#7593=DIRECTION('',(0.5,0.,0.866025403784439));
#7594=DIRECTION('',(0.,-1.,0.));
#7595=DIRECTION('center_axis',(1.20185167898973E-16,0.,-1.));
#7596=DIRECTION('ref_axis',(1.,0.,1.20185167898973E-16));
#7597=DIRECTION('',(-1.,0.,-1.20185167898973E-16));
#7598=DIRECTION('',(0.,-1.,0.));
#7599=DIRECTION('',(1.,0.,1.20185167898973E-16));
#7600=DIRECTION('center_axis',(-0.866025403784439,0.,-0.5));
#7601=DIRECTION('ref_axis',(0.5,0.,-0.866025403784439));
#7602=DIRECTION('',(-0.5,0.,0.866025403784439));
#7603=DIRECTION('',(0.,-1.,0.));
#7604=DIRECTION('',(0.5,0.,-0.866025403784439));
#7605=DIRECTION('center_axis',(-0.866025403784439,0.,0.5));
#7606=DIRECTION('ref_axis',(-0.5,0.,-0.866025403784439));
#7607=DIRECTION('',(0.5,0.,0.866025403784439));
#7608=DIRECTION('',(0.,-1.,0.));
#7609=DIRECTION('',(-0.5,0.,-0.866025403784439));
#7610=DIRECTION('center_axis',(-2.40370335797945E-16,0.,1.));
#7611=DIRECTION('ref_axis',(-1.,0.,-2.40370335797945E-16));
#7612=DIRECTION('',(1.,0.,2.40370335797945E-16));
#7613=DIRECTION('',(0.,-1.,0.));
#7614=DIRECTION('',(-1.,0.,-2.40370335797945E-16));
#7615=DIRECTION('center_axis',(0.866025403784439,0.,0.5));
#7616=DIRECTION('ref_axis',(-0.5,0.,0.866025403784439));
#7617=DIRECTION('',(0.5,0.,-0.866025403784439));
#7618=DIRECTION('',(-0.5,0.,0.866025403784439));
#7619=DIRECTION('center_axis',(0.,1.,0.));
#7620=DIRECTION('ref_axis',(1.,0.,0.));
#7621=DIRECTION('center_axis',(0.,-1.,0.));
#7622=DIRECTION('ref_axis',(0.,0.,-1.));
#7623=DIRECTION('center_axis',(0.,1.,0.));
#7624=DIRECTION('ref_axis',(1.,0.,0.));
#7625=DIRECTION('center_axis',(0.,1.,0.));
#7626=DIRECTION('ref_axis',(1.,0.,0.));
#7627=DIRECTION('center_axis',(0.,1.,0.));
#7628=DIRECTION('ref_axis',(1.,0.,0.));
#7629=DIRECTION('center_axis',(0.,1.,0.));
#7630=DIRECTION('ref_axis',(1.,0.,0.));
#7631=DIRECTION('',(0.,-1.,0.));
#7632=DIRECTION('center_axis',(0.,1.,0.));
#7633=DIRECTION('ref_axis',(1.,0.,0.));
#7634=DIRECTION('center_axis',(0.,1.,0.));
#7635=DIRECTION('ref_axis',(1.,0.,0.));
#7636=DIRECTION('center_axis',(0.,1.,0.));
#7637=DIRECTION('ref_axis',(0.,0.,1.));
#7638=DIRECTION('center_axis',(0.,-1.,0.));
#7639=DIRECTION('ref_axis',(1.,0.,0.));
#7640=DIRECTION('center_axis',(0.,-1.,0.));
#7641=DIRECTION('ref_axis',(1.,0.,0.));
#7642=DIRECTION('center_axis',(0.,-1.,0.));
#7643=DIRECTION('ref_axis',(1.,0.,0.));
#7644=DIRECTION('',(0.707106781186548,0.707106781186547,8.65956056235493E-17));
#7645=DIRECTION('center_axis',(0.,-1.,0.));
#7646=DIRECTION('ref_axis',(1.,0.,0.));
#7647=DIRECTION('center_axis',(0.,-1.,0.));
#7648=DIRECTION('ref_axis',(1.,0.,0.));
#7649=DIRECTION('',(0.,1.,0.));
#7650=DIRECTION('center_axis',(0.,1.,0.));
#7651=DIRECTION('ref_axis',(1.,0.,0.));
#7652=DIRECTION('center_axis',(0.,-1.,0.));
#7653=DIRECTION('ref_axis',(1.,0.,0.));
#7654=DIRECTION('',(-0.707106781186547,0.707106781186548,-8.65956056235493E-17));
#7655=DIRECTION('center_axis',(0.,-1.,0.));
#7656=DIRECTION('ref_axis',(0.,0.,-1.));
#7657=DIRECTION('center_axis',(0.,-1.,0.));
#7658=DIRECTION('ref_axis',(1.,0.,0.));
#7659=DIRECTION('center_axis',(0.,1.,0.));
#7660=DIRECTION('ref_axis',(1.,0.,0.));
#7661=DIRECTION('center_axis',(0.,1.,0.));
#7662=DIRECTION('ref_axis',(1.,0.,0.));
#7663=DIRECTION('',(-0.447213595499958,0.894427190999916,-5.47678698264203E-17));
#7664=DIRECTION('center_axis',(0.,-1.,0.));
#7665=DIRECTION('ref_axis',(1.,0.,0.));
#7666=DIRECTION('',(0.,1.,0.));
#7667=DIRECTION('axis',(0.,0.,1.));
#7668=DIRECTION('refdir',(1.,0.,0.));
#7669=DIRECTION('center_axis',(0.,1.,0.));
#7670=DIRECTION('ref_axis',(1.,0.,0.));
#7671=DIRECTION('center_axis',(0.,1.,0.));
#7672=DIRECTION('ref_axis',(1.,0.,0.));
#7673=DIRECTION('',(0.707106781186548,-0.707106781186547,-8.65956056235494E-17));
#7674=DIRECTION('center_axis',(0.,-1.,0.));
#7675=DIRECTION('ref_axis',(1.,0.,0.));
#7676=DIRECTION('center_axis',(0.,1.,0.));
#7677=DIRECTION('ref_axis',(1.,0.,0.));
#7678=DIRECTION('',(0.,-1.,0.));
#7679=DIRECTION('center_axis',(0.,-1.,0.));
#7680=DIRECTION('ref_axis',(1.,0.,0.));
#7681=DIRECTION('center_axis',(0.,1.,0.));
#7682=DIRECTION('ref_axis',(1.,0.,0.));
#7683=DIRECTION('center_axis',(0.,1.,0.));
#7684=DIRECTION('ref_axis',(1.,0.,0.));
#7685=DIRECTION('center_axis',(0.,1.,0.));
#7686=DIRECTION('ref_axis',(1.,0.,0.));
#7687=DIRECTION('',(0.,-1.,0.));
#7688=DIRECTION('center_axis',(0.,1.,0.));
#7689=DIRECTION('ref_axis',(1.,0.,0.));
#7690=DIRECTION('center_axis',(0.,1.,0.));
#7691=DIRECTION('ref_axis',(1.,0.,0.));
#7692=DIRECTION('axis',(0.,0.,1.));
#7693=DIRECTION('refdir',(1.,0.,0.));
#7694=DIRECTION('center_axis',(0.,1.,0.));
#7695=DIRECTION('ref_axis',(1.,0.,0.));
#7696=DIRECTION('',(0.866025403784439,-0.5,1.06057523872491E-16));
#7697=DIRECTION('center_axis',(0.,-1.,0.));
#7698=DIRECTION('ref_axis',(1.,0.,0.));
#7699=DIRECTION('center_axis',(0.,-1.,0.));
#7700=DIRECTION('ref_axis',(1.,0.,0.));
#7701=DIRECTION('center_axis',(0.,1.,0.));
#7702=DIRECTION('ref_axis',(1.,0.,0.));
#7703=DIRECTION('',(-0.866025403784439,-0.5,-1.06057523872491E-16));
#7704=DIRECTION('center_axis',(1.20185167898973E-16,0.,-1.));
#7705=DIRECTION('ref_axis',(-1.,0.,-1.20185167898973E-16));
#7706=DIRECTION('',(0.,1.,0.));
#7707=DIRECTION('',(0.,1.,0.));
#7708=DIRECTION('center_axis',(-0.866025403784439,0.,-0.5));
#7709=DIRECTION('ref_axis',(-0.5,0.,0.866025403784439));
#7710=DIRECTION('',(0.,1.,0.));
#7711=DIRECTION('center_axis',(-0.866025403784439,0.,0.5));
#7712=DIRECTION('ref_axis',(0.5,0.,0.866025403784439));
#7713=DIRECTION('',(0.,1.,0.));
#7714=DIRECTION('center_axis',(0.,1.,0.));
#7715=DIRECTION('ref_axis',(1.,0.,0.));
#7716=DIRECTION('center_axis',(0.,1.,0.));
#7717=DIRECTION('ref_axis',(1.,0.,0.));
#7718=DIRECTION('',(0.,-1.,0.));
#7719=DIRECTION('center_axis',(0.,1.,0.));
#7720=DIRECTION('ref_axis',(1.,0.,0.));
#7721=DIRECTION('center_axis',(-2.40370335797945E-16,0.,1.));
#7722=DIRECTION('ref_axis',(1.,0.,2.40370335797945E-16));
#7723=DIRECTION('',(0.,1.,0.));
#7724=DIRECTION('center_axis',(0.866025403784439,0.,-0.5));
#7725=DIRECTION('ref_axis',(-0.5,0.,-0.866025403784439));
#7726=DIRECTION('',(0.,1.,0.));
#7727=DIRECTION('center_axis',(0.866025403784439,0.,0.5));
#7728=DIRECTION('ref_axis',(0.5,0.,-0.866025403784439));
#7729=DIRECTION('center_axis',(0.,1.,0.));
#7730=DIRECTION('ref_axis',(1.,0.,0.));
#7731=DIRECTION('center_axis',(0.,1.,0.));
#7732=DIRECTION('ref_axis',(1.,0.,0.));
#7733=DIRECTION('axis',(0.,0.,1.));
#7734=DIRECTION('refdir',(1.,0.,0.));
#7735=DIRECTION('center_axis',(0.,1.,0.));
#7736=DIRECTION('ref_axis',(1.,0.,0.));
#7737=DIRECTION('',(-0.5,0.,0.866025403784439));
#7738=DIRECTION('',(-1.,0.,-2.84883360945713E-16));
#7739=DIRECTION('',(-0.5,0.,-0.866025403784439));
#7740=DIRECTION('',(0.5,0.,-0.866025403784439));
#7741=DIRECTION('',(1.,0.,0.));
#7742=DIRECTION('',(0.5,0.,0.866025403784439));
#7743=DIRECTION('center_axis',(0.,-1.,0.));
#7744=DIRECTION('ref_axis',(1.,0.,0.));
#7745=DIRECTION('center_axis',(0.,1.,0.));
#7746=DIRECTION('ref_axis',(1.,0.,0.));
#7747=DIRECTION('',(0.5,0.,-0.866025403784439));
#7748=DIRECTION('',(-0.5,0.,-0.866025403784439));
#7749=DIRECTION('',(-1.,0.,0.));
#7750=DIRECTION('',(-0.5,0.,0.866025403784439));
#7751=DIRECTION('',(0.5,0.,0.866025403784439));
#7752=DIRECTION('',(1.,0.,2.84883360945713E-16));
#7753=DIRECTION('center_axis',(0.,1.,0.));
#7754=DIRECTION('ref_axis',(1.,0.,0.));
#7755=DIRECTION('center_axis',(-2.84883360945713E-16,0.,1.));
#7756=DIRECTION('ref_axis',(1.,0.,2.84883360945713E-16));
#7757=DIRECTION('',(0.,-1.,0.));
#7758=DIRECTION('',(0.,1.,0.));
#7759=DIRECTION('center_axis',(-0.866025403784439,0.,0.5));
#7760=DIRECTION('ref_axis',(0.5,0.,0.866025403784439));
#7761=DIRECTION('',(0.,1.,0.));
#7762=DIRECTION('center_axis',(-0.866025403784439,0.,-0.5));
#7763=DIRECTION('ref_axis',(-0.5,0.,0.866025403784439));
#7764=DIRECTION('',(0.,1.,0.));
#7765=DIRECTION('center_axis',(0.,0.,-1.));
#7766=DIRECTION('ref_axis',(-1.,0.,0.));
#7767=DIRECTION('',(0.,1.,0.));
#7768=DIRECTION('center_axis',(0.866025403784439,0.,-0.5));
#7769=DIRECTION('ref_axis',(-0.5,0.,-0.866025403784439));
#7770=DIRECTION('',(0.,1.,0.));
#7771=DIRECTION('center_axis',(0.866025403784439,0.,0.5));
#7772=DIRECTION('ref_axis',(0.5,0.,-0.866025403784439));
#7773=DIRECTION('center_axis',(0.,-1.,0.));
#7774=DIRECTION('ref_axis',(1.,0.,0.));
#7775=DIRECTION('',(0.,1.,0.));
#7776=DIRECTION('center_axis',(0.,-1.,0.));
#7777=DIRECTION('ref_axis',(1.,0.,0.));
#7778=DIRECTION('center_axis',(0.,1.,0.));
#7779=DIRECTION('ref_axis',(0.,0.,1.));
#7780=DIRECTION('center_axis',(0.,-1.,0.));
#7781=DIRECTION('ref_axis',(1.,0.,0.));
#7782=DIRECTION('center_axis',(0.,-1.,0.));
#7783=DIRECTION('ref_axis',(1.,0.,0.));
#7784=DIRECTION('center_axis',(0.,-1.,0.));
#7785=DIRECTION('ref_axis',(1.,0.,0.));
#7786=DIRECTION('',(0.707106781186547,0.707106781186548,8.65956056235493E-17));
#7787=DIRECTION('center_axis',(0.,-1.,0.));
#7788=DIRECTION('ref_axis',(1.,0.,0.));
#7789=DIRECTION('center_axis',(0.,-1.,0.));
#7790=DIRECTION('ref_axis',(1.,0.,0.));
#7791=DIRECTION('',(0.,1.,0.));
#7792=DIRECTION('center_axis',(0.,1.,0.));
#7793=DIRECTION('ref_axis',(1.,0.,0.));
#7794=DIRECTION('center_axis',(0.,-1.,0.));
#7795=DIRECTION('ref_axis',(1.,0.,0.));
#7796=DIRECTION('',(-0.707106781186547,0.707106781186548,-8.65956056235493E-17));
#7797=DIRECTION('center_axis',(0.,-1.,0.));
#7798=DIRECTION('ref_axis',(0.,0.,-1.));
#7799=DIRECTION('center_axis',(0.,-1.,0.));
#7800=DIRECTION('ref_axis',(1.,0.,0.));
#7801=DIRECTION('center_axis',(0.,-1.,0.));
#7802=DIRECTION('ref_axis',(1.,0.,0.));
#7803=DIRECTION('',(0.,1.,0.));
#7804=DIRECTION('axis',(0.,0.,1.));
#7805=DIRECTION('refdir',(1.,0.,0.));
#7806=DIRECTION('center_axis',(0.,0.,1.));
#7807=DIRECTION('ref_axis',(1.,0.,0.));
#7808=DIRECTION('center_axis',(0.,0.,-1.));
#7809=DIRECTION('ref_axis',(1.,0.,0.));
#7810=DIRECTION('',(0.,0.,-1.));
#7811=DIRECTION('center_axis',(0.,0.,-1.));
#7812=DIRECTION('ref_axis',(1.,0.,0.));
#7813=DIRECTION('center_axis',(0.,0.,1.));
#7814=DIRECTION('ref_axis',(1.,0.,0.));
#7815=DIRECTION('center_axis',(0.,0.,1.));
#7816=DIRECTION('ref_axis',(1.,0.,0.));
#7817=DIRECTION('',(0.,0.,-1.));
#7818=DIRECTION('center_axis',(0.,0.,1.));
#7819=DIRECTION('ref_axis',(1.,0.,0.));
#7820=DIRECTION('center_axis',(0.,0.,1.));
#7821=DIRECTION('ref_axis',(1.,0.,0.));
#7822=DIRECTION('center_axis',(0.,0.,1.));
#7823=DIRECTION('ref_axis',(1.,0.,0.));
#7824=DIRECTION('axis',(0.,0.,1.));
#7825=DIRECTION('refdir',(1.,0.,0.));
#7826=DIRECTION('center_axis',(0.,1.,0.));
#7827=DIRECTION('ref_axis',(0.,0.,1.));
#7828=DIRECTION('center_axis',(0.,-1.,0.));
#7829=DIRECTION('ref_axis',(1.,0.,0.));
#7830=DIRECTION('center_axis',(0.,-1.,0.));
#7831=DIRECTION('ref_axis',(1.,0.,0.));
#7832=DIRECTION('center_axis',(0.,-1.,0.));
#7833=DIRECTION('ref_axis',(1.,0.,0.));
#7834=DIRECTION('',(0.707106781186547,0.707106781186548,8.65956056235493E-17));
#7835=DIRECTION('center_axis',(0.,-1.,0.));
#7836=DIRECTION('ref_axis',(1.,0.,0.));
#7837=DIRECTION('center_axis',(0.,-1.,0.));
#7838=DIRECTION('ref_axis',(1.,0.,0.));
#7839=DIRECTION('',(0.,1.,0.));
#7840=DIRECTION('center_axis',(0.,1.,0.));
#7841=DIRECTION('ref_axis',(1.,0.,0.));
#7842=DIRECTION('center_axis',(0.,-1.,0.));
#7843=DIRECTION('ref_axis',(1.,0.,0.));
#7844=DIRECTION('',(-0.707106781186547,0.707106781186548,-8.65956056235493E-17));
#7845=DIRECTION('center_axis',(0.,-1.,0.));
#7846=DIRECTION('ref_axis',(0.,0.,-1.));
#7847=DIRECTION('center_axis',(0.,-1.,0.));
#7848=DIRECTION('ref_axis',(1.,0.,0.));
#7849=DIRECTION('center_axis',(0.,1.,0.));
#7850=DIRECTION('ref_axis',(1.,0.,0.));
#7851=DIRECTION('center_axis',(0.,1.,0.));
#7852=DIRECTION('ref_axis',(1.,0.,0.));
#7853=DIRECTION('',(-0.447213595499958,0.894427190999916,-5.47678698264203E-17));
#7854=DIRECTION('center_axis',(0.,-1.,0.));
#7855=DIRECTION('ref_axis',(1.,0.,0.));
#7856=DIRECTION('center_axis',(0.,1.,0.));
#7857=DIRECTION('ref_axis',(1.,0.,0.));
#7858=DIRECTION('',(0.,1.,0.));
#7859=DIRECTION('center_axis',(0.,1.,0.));
#7860=DIRECTION('ref_axis',(1.,0.,0.));
#7861=DIRECTION('center_axis',(0.,-1.,0.));
#7862=DIRECTION('ref_axis',(1.,0.,0.));
#7863=DIRECTION('',(-0.707106781186547,0.707106781186548,-8.65956056235493E-17));
#7864=DIRECTION('center_axis',(0.,-1.,0.));
#7865=DIRECTION('ref_axis',(0.,0.,-1.));
#7866=DIRECTION('center_axis',(0.866025403784439,0.,-0.5));
#7867=DIRECTION('ref_axis',(0.5,0.,0.866025403784439));
#7868=DIRECTION('',(-0.5,0.,-0.866025403784439));
#7869=DIRECTION('',(0.,-1.,0.));
#7870=DIRECTION('',(0.5,0.,0.866025403784439));
#7871=DIRECTION('',(0.,-1.,0.));
#7872=DIRECTION('center_axis',(1.60246890531964E-16,0.,-1.));
#7873=DIRECTION('ref_axis',(1.,0.,1.60246890531964E-16));
#7874=DIRECTION('',(-1.,0.,-1.60246890531964E-16));
#7875=DIRECTION('',(0.,-1.,0.));
#7876=DIRECTION('',(1.,0.,1.60246890531964E-16));
#7877=DIRECTION('center_axis',(-0.866025403784439,0.,-0.5));
#7878=DIRECTION('ref_axis',(0.5,0.,-0.866025403784439));
#7879=DIRECTION('',(-0.5,0.,0.866025403784439));
#7880=DIRECTION('',(0.,-1.,0.));
#7881=DIRECTION('',(0.5,0.,-0.866025403784439));
#7882=DIRECTION('center_axis',(-0.866025403784439,0.,0.5));
#7883=DIRECTION('ref_axis',(-0.5,0.,-0.866025403784439));
#7884=DIRECTION('',(0.5,0.,0.866025403784439));
#7885=DIRECTION('',(0.,-1.,0.));
#7886=DIRECTION('',(-0.5,0.,-0.866025403784439));
#7887=DIRECTION('center_axis',(-1.60246890531964E-16,0.,1.));
#7888=DIRECTION('ref_axis',(-1.,0.,-1.60246890531964E-16));
#7889=DIRECTION('',(1.,0.,1.60246890531964E-16));
#7890=DIRECTION('',(0.,-1.,0.));
#7891=DIRECTION('',(-1.,0.,-1.60246890531964E-16));
#7892=DIRECTION('center_axis',(0.866025403784439,0.,0.5));
#7893=DIRECTION('ref_axis',(-0.5,0.,0.866025403784439));
#7894=DIRECTION('',(0.5,0.,-0.866025403784439));
#7895=DIRECTION('',(-0.5,0.,0.866025403784439));
#7896=DIRECTION('center_axis',(0.,1.,0.));
#7897=DIRECTION('ref_axis',(1.,0.,0.));
#7898=DIRECTION('center_axis',(0.,-1.,0.));
#7899=DIRECTION('ref_axis',(0.,0.,-1.));
#7900=DIRECTION('axis',(0.,0.,1.));
#7901=DIRECTION('refdir',(1.,0.,0.));
#7902=DIRECTION('center_axis',(0.,0.,1.));
#7903=DIRECTION('ref_axis',(1.,0.,0.));
#7904=DIRECTION('center_axis',(0.,0.,1.));
#7905=DIRECTION('ref_axis',(1.,0.,0.));
#7906=DIRECTION('',(0.,0.,-1.));
#7907=DIRECTION('center_axis',(0.,0.,1.));
#7908=DIRECTION('ref_axis',(1.,0.,0.));
#7909=DIRECTION('center_axis',(0.,0.,1.));
#7910=DIRECTION('ref_axis',(1.,0.,0.));
#7911=DIRECTION('center_axis',(0.,0.,1.));
#7912=DIRECTION('ref_axis',(1.,0.,0.));
#7913=DIRECTION('axis',(0.,0.,1.));
#7914=DIRECTION('refdir',(1.,0.,0.));
#7915=DIRECTION('axis',(0.,0.,1.));
#7916=DIRECTION('refdir',(1.,0.,0.));
#7917=DIRECTION('center_axis',(0.,-1.,0.));
#7918=DIRECTION('ref_axis',(1.,0.,0.));
#7919=DIRECTION('center_axis',(0.,-1.,0.));
#7920=DIRECTION('ref_axis',(0.,0.,1.));
#7921=DIRECTION('',(0.,0.,1.));
#7922=DIRECTION('',(1.,0.,0.));
#7923=DIRECTION('',(0.,0.,1.));
#7924=DIRECTION('center_axis',(-1.,0.,0.));
#7925=DIRECTION('ref_axis',(0.,-1.,0.));
#7926=DIRECTION('center_axis',(-1.,0.,0.));
#7927=DIRECTION('ref_axis',(0.,0.,-1.));
#7928=DIRECTION('',(0.,-1.,0.));
#7929=DIRECTION('',(0.,0.,1.));
#7930=DIRECTION('center_axis',(-1.,0.,0.));
#7931=DIRECTION('ref_axis',(0.,0.,-1.));
#7932=DIRECTION('center_axis',(0.,1.,0.));
#7933=DIRECTION('ref_axis',(-1.,0.,0.));
#7934=DIRECTION('center_axis',(0.,1.,0.));
#7935=DIRECTION('ref_axis',(0.,0.,-1.));
#7936=DIRECTION('',(-1.,0.,0.));
#7937=DIRECTION('',(0.,0.,1.));
#7938=DIRECTION('center_axis',(1.,0.,0.));
#7939=DIRECTION('ref_axis',(0.,1.,0.));
#7940=DIRECTION('center_axis',(1.,0.,0.));
#7941=DIRECTION('ref_axis',(0.,0.,1.));
#7942=DIRECTION('',(0.,1.,0.));
#7943=DIRECTION('center_axis',(0.,0.,1.));
#7944=DIRECTION('ref_axis',(1.,0.,0.));
#7945=DIRECTION('center_axis',(0.,1.,0.));
#7946=DIRECTION('ref_axis',(1.,0.,0.));
#7947=DIRECTION('center_axis',(0.,1.,0.));
#7948=DIRECTION('ref_axis',(1.,0.,0.));
#7949=DIRECTION('',(0.,1.,0.));
#7950=DIRECTION('center_axis',(0.,-1.,0.));
#7951=DIRECTION('ref_axis',(1.,0.,0.));
#7952=DIRECTION('center_axis',(6.12323399573677E-17,0.,1.));
#7953=DIRECTION('ref_axis',(1.,0.,0.));
#7954=DIRECTION('center_axis',(1.22464679914735E-16,-1.,0.));
#7955=DIRECTION('ref_axis',(-1.,-1.22464679914735E-16,0.));
#7956=DIRECTION('axis',(0.,0.,1.));
#7957=DIRECTION('refdir',(1.,0.,0.));
#7958=DIRECTION('center_axis',(0.,0.,1.));
#7959=DIRECTION('ref_axis',(1.,0.,0.));
#7960=DIRECTION('center_axis',(0.,0.,1.));
#7961=DIRECTION('ref_axis',(1.,0.,0.));
#7962=DIRECTION('',(0.,0.,1.));
#7963=DIRECTION('center_axis',(0.,0.,-1.));
#7964=DIRECTION('ref_axis',(1.,0.,0.));
#7965=DIRECTION('center_axis',(0.,0.,1.));
#7966=DIRECTION('ref_axis',(1.,0.,0.));
#7967=DIRECTION('center_axis',(0.,0.,1.));
#7968=DIRECTION('ref_axis',(1.,0.,0.));
#7969=DIRECTION('center_axis',(0.,0.,1.));
#7970=DIRECTION('ref_axis',(1.,0.,0.));
#7971=DIRECTION('',(0.,-1.,0.));
#7972=DIRECTION('',(-1.,0.,0.));
#7973=DIRECTION('center_axis',(0.,0.,1.));
#7974=DIRECTION('ref_axis',(1.,0.,0.));
#7975=DIRECTION('center_axis',(0.,0.,1.));
#7976=DIRECTION('ref_axis',(1.,0.,0.));
#7977=DIRECTION('',(1.,0.,0.));
#7978=DIRECTION('',(0.,-1.,0.));
#7979=DIRECTION('center_axis',(0.,0.,1.));
#7980=DIRECTION('ref_axis',(1.,0.,0.));
#7981=DIRECTION('center_axis',(0.,0.,1.));
#7982=DIRECTION('ref_axis',(1.,0.,0.));
#7983=DIRECTION('',(0.,1.,0.));
#7984=DIRECTION('',(1.,0.,0.));
#7985=DIRECTION('center_axis',(0.,0.,1.));
#7986=DIRECTION('ref_axis',(1.,0.,0.));
#7987=DIRECTION('center_axis',(0.,0.,1.));
#7988=DIRECTION('ref_axis',(1.,0.,0.));
#7989=DIRECTION('',(-1.,0.,0.));
#7990=DIRECTION('',(0.,1.,0.));
#7991=DIRECTION('center_axis',(0.,1.,0.));
#7992=DIRECTION('ref_axis',(-1.,0.,0.));
#7993=DIRECTION('',(1.,0.,0.));
#7994=DIRECTION('',(0.,0.,1.));
#7995=DIRECTION('',(-1.,0.,0.));
#7996=DIRECTION('',(0.,0.,1.));
#7997=DIRECTION('center_axis',(1.,0.,0.));
#7998=DIRECTION('ref_axis',(0.,1.,0.));
#7999=DIRECTION('',(0.,-1.,0.));
#8000=DIRECTION('',(0.,1.,0.));
#8001=DIRECTION('',(0.,0.,1.));
#8002=DIRECTION('center_axis',(0.,-1.,0.));
#8003=DIRECTION('ref_axis',(1.,0.,0.));
#8004=DIRECTION('',(-1.,0.,0.));
#8005=DIRECTION('',(1.,0.,0.));
#8006=DIRECTION('',(0.,0.,1.));
#8007=DIRECTION('center_axis',(-1.,0.,0.));
#8008=DIRECTION('ref_axis',(0.,-1.,0.));
#8009=DIRECTION('',(0.,1.,0.));
#8010=DIRECTION('',(0.,-1.,0.));
#8011=DIRECTION('center_axis',(0.,0.,1.));
#8012=DIRECTION('ref_axis',(1.,0.,0.));
#8013=DIRECTION('center_axis',(0.,0.,1.));
#8014=DIRECTION('ref_axis',(1.,0.,0.));
#8015=DIRECTION('center_axis',(0.,0.,1.));
#8016=DIRECTION('ref_axis',(1.,0.,0.));
#8017=DIRECTION('center_axis',(0.,0.,1.));
#8018=DIRECTION('ref_axis',(1.,0.,0.));
#8019=DIRECTION('center_axis',(0.,0.,1.));
#8020=DIRECTION('ref_axis',(1.,0.,0.));
#8021=DIRECTION('center_axis',(0.,0.,1.));
#8022=DIRECTION('ref_axis',(1.,0.,0.));
#8023=DIRECTION('center_axis',(0.,0.,1.));
#8024=DIRECTION('ref_axis',(1.,0.,0.));
#8025=DIRECTION('center_axis',(0.,0.,1.));
#8026=DIRECTION('ref_axis',(1.,0.,0.));
#8027=DIRECTION('center_axis',(0.,0.,1.));
#8028=DIRECTION('ref_axis',(1.,0.,0.));
#8029=DIRECTION('center_axis',(0.,0.,1.));
#8030=DIRECTION('ref_axis',(1.,0.,0.));
#8031=DIRECTION('center_axis',(0.,1.,0.));
#8032=DIRECTION('ref_axis',(-1.,0.,0.));
#8033=DIRECTION('',(-1.,0.,0.));
#8034=DIRECTION('',(0.,0.,1.));
#8035=DIRECTION('',(-1.,0.,0.));
#8036=DIRECTION('',(0.,0.,1.));
#8037=DIRECTION('center_axis',(1.,0.,0.));
#8038=DIRECTION('ref_axis',(0.,1.,0.));
#8039=DIRECTION('',(0.,1.,0.));
#8040=DIRECTION('',(0.,1.,0.));
#8041=DIRECTION('',(0.,0.,1.));
#8042=DIRECTION('center_axis',(0.,-1.,0.));
#8043=DIRECTION('ref_axis',(1.,0.,0.));
#8044=DIRECTION('',(1.,0.,0.));
#8045=DIRECTION('',(1.,0.,0.));
#8046=DIRECTION('',(0.,0.,1.));
#8047=DIRECTION('center_axis',(-1.,0.,0.));
#8048=DIRECTION('ref_axis',(0.,-1.,0.));
#8049=DIRECTION('',(0.,-1.,0.));
#8050=DIRECTION('',(0.,-1.,0.));
#8051=DIRECTION('center_axis',(0.,0.,1.));
#8052=DIRECTION('ref_axis',(1.,0.,0.));
#8053=DIRECTION('center_axis',(0.,0.,1.));
#8054=DIRECTION('ref_axis',(1.,0.,0.));
#8055=DIRECTION('',(0.,0.,-1.));
#8056=DIRECTION('center_axis',(0.,0.,1.));
#8057=DIRECTION('ref_axis',(1.,0.,0.));
#8058=DIRECTION('center_axis',(0.,0.,1.));
#8059=DIRECTION('ref_axis',(1.,0.,0.));
#8060=DIRECTION('axis',(0.,0.,1.));
#8061=DIRECTION('refdir',(1.,0.,0.));
#8062=DIRECTION('center_axis',(0.,-1.,0.));
#8063=DIRECTION('ref_axis',(1.,0.,0.));
#8064=DIRECTION('',(-1.,0.,0.));
#8065=DIRECTION('',(0.,0.,1.));
#8066=DIRECTION('',(1.,0.,0.));
#8067=DIRECTION('',(0.,0.,1.));
#8068=DIRECTION('center_axis',(-1.,0.,0.));
#8069=DIRECTION('ref_axis',(0.,-1.,0.));
#8070=DIRECTION('',(0.,1.,0.));
#8071=DIRECTION('',(0.,-1.,0.));
#8072=DIRECTION('',(0.,0.,1.));
#8073=DIRECTION('center_axis',(0.,1.,0.));
#8074=DIRECTION('ref_axis',(-1.,0.,0.));
#8075=DIRECTION('',(1.,0.,0.));
#8076=DIRECTION('',(-1.,0.,0.));
#8077=DIRECTION('',(0.,0.,1.));
#8078=DIRECTION('center_axis',(1.,0.,0.));
#8079=DIRECTION('ref_axis',(0.,1.,0.));
#8080=DIRECTION('',(0.,-1.,0.));
#8081=DIRECTION('',(0.,1.,0.));
#8082=DIRECTION('center_axis',(0.,1.,0.));
#8083=DIRECTION('ref_axis',(-1.,0.,0.));
#8084=DIRECTION('',(-1.,0.,0.));
#8085=DIRECTION('',(0.,0.,1.));
#8086=DIRECTION('',(-1.,0.,0.));
#8087=DIRECTION('',(0.,0.,1.));
#8088=DIRECTION('center_axis',(1.,0.,0.));
#8089=DIRECTION('ref_axis',(0.,1.,0.));
#8090=DIRECTION('',(0.,1.,0.));
#8091=DIRECTION('',(0.,1.,0.));
#8092=DIRECTION('',(0.,0.,1.));
#8093=DIRECTION('center_axis',(0.,-1.,0.));
#8094=DIRECTION('ref_axis',(1.,0.,0.));
#8095=DIRECTION('',(1.,0.,0.));
#8096=DIRECTION('',(1.,0.,0.));
#8097=DIRECTION('',(0.,0.,1.));
#8098=DIRECTION('center_axis',(-1.,0.,0.));
#8099=DIRECTION('ref_axis',(0.,-1.,0.));
#8100=DIRECTION('',(0.,-1.,0.));
#8101=DIRECTION('',(0.,-1.,0.));
#8102=DIRECTION('center_axis',(0.,0.,1.));
#8103=DIRECTION('ref_axis',(1.,0.,0.));
#8104=DIRECTION('center_axis',(0.,0.,1.));
#8105=DIRECTION('ref_axis',(1.,0.,0.));
#8106=DIRECTION('axis',(0.,0.,1.));
#8107=DIRECTION('refdir',(1.,0.,0.));
#8108=DIRECTION('center_axis',(0.,0.,1.));
#8109=DIRECTION('ref_axis',(1.,0.,0.));
#8110=DIRECTION('center_axis',(0.,0.,-1.));
#8111=DIRECTION('ref_axis',(1.,0.,0.));
#8112=DIRECTION('',(0.,0.,-1.));
#8113=DIRECTION('center_axis',(0.,0.,-1.));
#8114=DIRECTION('ref_axis',(1.,0.,0.));
#8115=DIRECTION('center_axis',(0.,0.,1.));
#8116=DIRECTION('ref_axis',(1.,0.,0.));
#8117=DIRECTION('center_axis',(0.,0.,1.));
#8118=DIRECTION('ref_axis',(1.,0.,0.));
#8119=DIRECTION('',(0.,0.,-1.));
#8120=DIRECTION('center_axis',(0.,0.,1.));
#8121=DIRECTION('ref_axis',(1.,0.,0.));
#8122=DIRECTION('center_axis',(0.,0.,1.));
#8123=DIRECTION('ref_axis',(1.,0.,0.));
#8124=DIRECTION('center_axis',(0.,0.,1.));
#8125=DIRECTION('ref_axis',(1.,0.,0.));
#8126=DIRECTION('axis',(0.,0.,1.));
#8127=DIRECTION('refdir',(1.,0.,0.));
#8128=DIRECTION('center_axis',(0.,1.,0.));
#8129=DIRECTION('ref_axis',(-1.,0.,0.));
#8130=DIRECTION('',(-1.,0.,0.));
#8131=DIRECTION('',(0.,0.,1.));
#8132=DIRECTION('',(-1.,0.,0.));
#8133=DIRECTION('',(0.,0.,1.));
#8134=DIRECTION('center_axis',(1.,0.,0.));
#8135=DIRECTION('ref_axis',(0.,1.,0.));
#8136=DIRECTION('',(0.,1.,0.));
#8137=DIRECTION('',(0.,1.,0.));
#8138=DIRECTION('',(0.,0.,1.));
#8139=DIRECTION('center_axis',(0.,-1.,0.));
#8140=DIRECTION('ref_axis',(1.,0.,0.));
#8141=DIRECTION('',(1.,0.,0.));
#8142=DIRECTION('',(1.,0.,0.));
#8143=DIRECTION('',(0.,0.,1.));
#8144=DIRECTION('center_axis',(-1.,0.,0.));
#8145=DIRECTION('ref_axis',(0.,-1.,0.));
#8146=DIRECTION('',(0.,-1.,0.));
#8147=DIRECTION('',(0.,-1.,0.));
#8148=DIRECTION('center_axis',(0.,0.,1.));
#8149=DIRECTION('ref_axis',(1.,0.,0.));
#8150=DIRECTION('center_axis',(0.,0.,1.));
#8151=DIRECTION('ref_axis',(1.,0.,0.));
#8152=DIRECTION('axis',(0.,0.,1.));
#8153=DIRECTION('refdir',(1.,0.,0.));
#8154=DIRECTION('center_axis',(0.866025403784439,0.,-0.5));
#8155=DIRECTION('ref_axis',(0.5,0.,0.866025403784439));
#8156=DIRECTION('',(-0.5,0.,-0.866025403784439));
#8157=DIRECTION('',(0.,-1.,0.));
#8158=DIRECTION('',(0.5,0.,0.866025403784439));
#8159=DIRECTION('',(0.,-1.,0.));
#8160=DIRECTION('center_axis',(1.60246890531964E-16,0.,-1.));
#8161=DIRECTION('ref_axis',(1.,0.,1.60246890531964E-16));
#8162=DIRECTION('',(-1.,0.,-1.60246890531964E-16));
#8163=DIRECTION('',(0.,-1.,0.));
#8164=DIRECTION('',(1.,0.,1.60246890531964E-16));
#8165=DIRECTION('center_axis',(-0.866025403784439,0.,-0.5));
#8166=DIRECTION('ref_axis',(0.5,0.,-0.866025403784439));
#8167=DIRECTION('',(-0.5,0.,0.866025403784439));
#8168=DIRECTION('',(0.,-1.,0.));
#8169=DIRECTION('',(0.5,0.,-0.866025403784439));
#8170=DIRECTION('center_axis',(-0.866025403784439,0.,0.5));
#8171=DIRECTION('ref_axis',(-0.5,0.,-0.866025403784439));
#8172=DIRECTION('',(0.5,0.,0.866025403784439));
#8173=DIRECTION('',(0.,-1.,0.));
#8174=DIRECTION('',(-0.5,0.,-0.866025403784439));
#8175=DIRECTION('center_axis',(-1.60246890531964E-16,0.,1.));
#8176=DIRECTION('ref_axis',(-1.,0.,-1.60246890531964E-16));
#8177=DIRECTION('',(1.,0.,1.60246890531964E-16));
#8178=DIRECTION('',(0.,-1.,0.));
#8179=DIRECTION('',(-1.,0.,-1.60246890531964E-16));
#8180=DIRECTION('center_axis',(0.866025403784439,0.,0.5));
#8181=DIRECTION('ref_axis',(-0.5,0.,0.866025403784439));
#8182=DIRECTION('',(0.5,0.,-0.866025403784439));
#8183=DIRECTION('',(-0.5,0.,0.866025403784439));
#8184=DIRECTION('center_axis',(0.,1.,0.));
#8185=DIRECTION('ref_axis',(1.,0.,0.));
#8186=DIRECTION('center_axis',(0.,-1.,0.));
#8187=DIRECTION('ref_axis',(0.,0.,-1.));
#8188=DIRECTION('center_axis',(0.,1.,0.));
#8189=DIRECTION('ref_axis',(1.,0.,0.));
#8190=DIRECTION('center_axis',(0.,1.,0.));
#8191=DIRECTION('ref_axis',(1.,0.,0.));
#8192=DIRECTION('center_axis',(0.,1.,0.));
#8193=DIRECTION('ref_axis',(0.,0.,1.));
#8194=DIRECTION('center_axis',(0.,-1.,0.));
#8195=DIRECTION('ref_axis',(1.,0.,0.));
#8196=DIRECTION('center_axis',(0.,-1.,0.));
#8197=DIRECTION('ref_axis',(1.,0.,0.));
#8198=DIRECTION('center_axis',(0.,-1.,0.));
#8199=DIRECTION('ref_axis',(1.,0.,0.));
#8200=DIRECTION('',(0.707106781186547,0.707106781186548,8.65956056235493E-17));
#8201=DIRECTION('center_axis',(0.,-1.,0.));
#8202=DIRECTION('ref_axis',(1.,0.,0.));
#8203=DIRECTION('center_axis',(0.,-1.,0.));
#8204=DIRECTION('ref_axis',(1.,0.,0.));
#8205=DIRECTION('',(0.,1.,0.));
#8206=DIRECTION('center_axis',(0.,1.,0.));
#8207=DIRECTION('ref_axis',(1.,0.,0.));
#8208=DIRECTION('center_axis',(0.,-1.,0.));
#8209=DIRECTION('ref_axis',(1.,0.,0.));
#8210=DIRECTION('',(-0.707106781186547,0.707106781186548,-8.65956056235493E-17));
#8211=DIRECTION('center_axis',(0.,-1.,0.));
#8212=DIRECTION('ref_axis',(0.,0.,-1.));
#8213=DIRECTION('center_axis',(0.,-1.,0.));
#8214=DIRECTION('ref_axis',(1.,0.,0.));
#8215=DIRECTION('center_axis',(0.,1.,0.));
#8216=DIRECTION('ref_axis',(1.,0.,0.));
#8217=DIRECTION('center_axis',(0.,1.,0.));
#8218=DIRECTION('ref_axis',(1.,0.,0.));
#8219=DIRECTION('',(-0.447213595499958,0.894427190999916,-5.47678698264203E-17));
#8220=DIRECTION('center_axis',(0.,-1.,0.));
#8221=DIRECTION('ref_axis',(1.,0.,0.));
#8222=DIRECTION('',(0.,1.,0.));
#8223=DIRECTION('',(0.,0.,1.));
#8224=DIRECTION('',(1.,0.,0.));
#8225=DIRECTION('',(0.,0.,1.));
#8226=DIRECTION('',(1.,0.,0.));
#8227=DIRECTION('',(0.,0.,1.));
#8228=DIRECTION('',(1.,0.,0.));
#8229=DIRECTION('',(0.,0.,1.));
#8230=DIRECTION('',(1.,0.,0.));
#8231=DIRECTION('',(0.,0.,1.));
#8232=DIRECTION('',(1.,0.,0.));
#8233=DIRECTION('',(0.,-1.,2.22044604925031E-16));
#8234=DIRECTION('',(1.,0.,0.));
#8235=DIRECTION('',(0.,0.,1.));
#8236=DIRECTION('',(1.,0.,0.));
#8237=DIRECTION('',(0.,0.,1.));
#8238=DIRECTION('',(1.,0.,0.));
#8239=DIRECTION('',(0.,0.,1.));
#8240=DIRECTION('',(1.,0.,0.));
#8241=DIRECTION('',(0.,0.,1.));
#8242=DIRECTION('',(1.,0.,0.));
#8243=DIRECTION('',(0.,0.,1.));
#8244=DIRECTION('',(1.,0.,0.));
#8245=DIRECTION('',(0.,0.,1.));
#8246=DIRECTION('',(1.,0.,0.));
#8247=DIRECTION('',(0.,0.,1.));
#8248=DIRECTION('',(1.,0.,0.));
#8249=DIRECTION('',(0.,0.,1.));
#8250=DIRECTION('',(1.,0.,0.));
#8251=DIRECTION('',(0.,0.,1.));
#8252=DIRECTION('',(-1.,1.22464679914735E-16,0.));
#8253=DIRECTION('',(0.,0.,1.));
#8254=DIRECTION('',(-1.,1.22464679914735E-16,0.));
#8255=DIRECTION('',(0.,0.,1.));
#8256=DIRECTION('',(-1.,1.22464679914735E-16,0.));
#8257=DIRECTION('',(0.,0.,1.));
#8258=DIRECTION('',(1.,0.,0.));
#8259=DIRECTION('',(0.,0.,1.));
#8260=DIRECTION('',(1.,0.,0.));
#8261=DIRECTION('',(0.,0.,1.));
#8262=DIRECTION('',(-1.,1.22464679914735E-16,0.));
#8263=DIRECTION('',(0.,0.,1.));
#8264=DIRECTION('',(-1.,1.22464679914735E-16,0.));
#8265=DIRECTION('',(0.,0.,1.));
#8266=DIRECTION('',(1.,0.,0.));
#8267=DIRECTION('',(0.,0.,1.));
#8268=DIRECTION('',(1.,0.,0.));
#8269=DIRECTION('',(0.,0.,1.));
#8270=DIRECTION('',(-1.,1.22464679914735E-16,0.));
#8271=DIRECTION('',(0.,0.,1.));
#8272=DIRECTION('',(-1.,1.22464679914735E-16,0.));
#8273=DIRECTION('',(0.,0.,1.));
#8274=DIRECTION('',(1.,0.,0.));
#8275=DIRECTION('',(0.,0.,1.));
#8276=DIRECTION('',(1.,0.,0.));
#8277=DIRECTION('',(0.,0.,1.));
#8278=DIRECTION('',(-1.,1.22464679914735E-16,0.));
#8279=DIRECTION('',(0.,0.,1.));
#8280=DIRECTION('',(-1.,1.22464679914735E-16,0.));
#8281=DIRECTION('',(0.,0.,1.));
#8282=DIRECTION('',(1.,0.,0.));
#8283=DIRECTION('',(0.,0.,1.));
#8284=DIRECTION('',(1.,0.,0.));
#8285=DIRECTION('',(0.,0.,1.));
#8286=DIRECTION('',(1.,0.,0.));
#8287=DIRECTION('',(0.,0.,1.));
#8288=DIRECTION('',(1.,0.,0.));
#8289=DIRECTION('',(0.,0.,1.));
#8290=DIRECTION('',(1.,0.,0.));
#8291=DIRECTION('',(0.,-1.,2.22044604925031E-16));
#8292=DIRECTION('',(1.,0.,0.));
#8293=DIRECTION('',(0.,0.,1.));
#8294=DIRECTION('',(1.,0.,0.));
#8295=DIRECTION('',(0.,-1.,2.22044604925031E-16));
#8296=DIRECTION('',(1.,0.,0.));
#8297=DIRECTION('',(0.,0.,1.));
#8298=DIRECTION('',(1.,0.,0.));
#8299=DIRECTION('',(0.,-1.,2.22044604925031E-16));
#8300=DIRECTION('',(1.,0.,0.));
#8301=DIRECTION('',(0.,0.,1.));
#8302=DIRECTION('',(1.,0.,0.));
#8303=DIRECTION('',(0.,-1.,2.22044604925031E-16));
#8304=DIRECTION('',(1.,0.,0.));
#8305=DIRECTION('',(0.,0.,1.));
#8306=DIRECTION('',(1.,0.,0.));
#8307=DIRECTION('',(0.,0.,1.));
#8308=DIRECTION('',(1.,0.,0.));
#8309=DIRECTION('',(0.,0.,1.));
#8310=DIRECTION('',(1.,0.,0.));
#8311=DIRECTION('',(0.,0.,1.));
#8312=DIRECTION('',(1.,0.,0.));
#8313=DIRECTION('',(0.,0.,1.));
#8314=DIRECTION('',(1.,0.,0.));
#8315=DIRECTION('',(0.,0.,1.));
#8316=DIRECTION('',(1.,0.,0.));
#8317=DIRECTION('',(0.,0.,1.));
#8318=DIRECTION('',(1.,0.,0.));
#8319=DIRECTION('',(0.,0.,1.));
#8320=DIRECTION('',(1.,0.,0.));
#8321=DIRECTION('',(0.,0.,1.));
#8322=DIRECTION('',(2.22044604925031E-16,-1.,0.));
#8323=DIRECTION('',(0.,1.,2.22044604925031E-16));
#8324=DIRECTION('',(1.,0.,0.));
#8325=DIRECTION('',(0.,1.,2.22044604925031E-16));
#8326=DIRECTION('',(1.,0.,0.));
#8327=DIRECTION('',(0.,0.,1.));
#8328=DIRECTION('',(1.,0.,0.));
#8329=DIRECTION('',(1.23259516440783E-32,0.,1.));
#8330=DIRECTION('',(1.,1.11022302462516E-16,1.11022302462516E-16));
#8331=DIRECTION('',(0.,0.,1.));
#8332=DIRECTION('',(1.,0.,0.));
#8333=DIRECTION('',(0.,0.,1.));
#8334=DIRECTION('',(1.,0.,0.));
#8335=CARTESIAN_POINT('',(0.,0.,0.));
#8336=CARTESIAN_POINT('',(0.,0.,0.));
#8337=CARTESIAN_POINT('',(0.,0.,0.));
#8338=CARTESIAN_POINT('Origin',(38.5,9.,3.4));
#8339=CARTESIAN_POINT('',(38.25,9.,3.5));
#8340=CARTESIAN_POINT('Origin',(38.5,9.,3.5));
#8341=CARTESIAN_POINT('',(38.25,9.,5.3));
#8342=CARTESIAN_POINT('',(38.25,9.,3.4));
#8343=CARTESIAN_POINT('Origin',(38.5,9.,5.3));
#8344=CARTESIAN_POINT('Origin',(38.5,9.,5.3));
#8345=CARTESIAN_POINT('Origin',(-2.5,9.,3.4));
#8346=CARTESIAN_POINT('',(-2.75,9.,3.5));
#8347=CARTESIAN_POINT('Origin',(-2.5,9.,3.5));
#8348=CARTESIAN_POINT('',(-2.75,9.,5.3));
#8349=CARTESIAN_POINT('',(-2.75,9.,3.4));
#8350=CARTESIAN_POINT('Origin',(-2.5,9.,5.3));
#8351=CARTESIAN_POINT('Origin',(-2.5,9.,5.3));
#8352=CARTESIAN_POINT('Origin',(38.7,7.75,5.));
#8353=CARTESIAN_POINT('',(38.7,7.75,5.93));
#8354=CARTESIAN_POINT('Origin',(38.7,7.75,5.));
#8355=CARTESIAN_POINT('',(40.,7.75,5.93));
#8356=CARTESIAN_POINT('',(38.7,7.75,5.93));
#8357=CARTESIAN_POINT('Origin',(40.,7.75,5.));
#8358=CARTESIAN_POINT('Origin',(38.7,7.75,5.));
#8359=CARTESIAN_POINT('',(38.7,7.75,5.79));
#8360=CARTESIAN_POINT('Origin',(38.7,7.75,5.));
#8361=CARTESIAN_POINT('Origin',(-4.1,7.75,5.));
#8362=CARTESIAN_POINT('',(-4.,7.75,5.93));
#8363=CARTESIAN_POINT('Origin',(-4.,7.75,5.));
#8364=CARTESIAN_POINT('',(-2.7,7.75,5.93));
#8365=CARTESIAN_POINT('',(-4.1,7.75,5.93));
#8366=CARTESIAN_POINT('Origin',(-2.7,7.75,5.));
#8367=CARTESIAN_POINT('Origin',(-2.7,7.75,5.));
#8368=CARTESIAN_POINT('',(-2.7,7.75,5.79));
#8369=CARTESIAN_POINT('Origin',(-2.7,7.75,5.));
#8370=CARTESIAN_POINT('Origin',(36.,7.9,5.));
#8371=CARTESIAN_POINT('',(35.85,7.9,4.22437122281339));
#8372=CARTESIAN_POINT('',(36.15,7.9,4.22437122281339));
#8373=CARTESIAN_POINT('',(-4.1,7.9,4.22437122281339));
#8374=CARTESIAN_POINT('Origin',(36.,7.9,5.));
#8375=CARTESIAN_POINT('Origin',(36.,7.2,5.));
#8376=CARTESIAN_POINT('',(36.,7.75,4.21));
#8377=CARTESIAN_POINT('Origin',(36.,7.75,5.));
#8378=CARTESIAN_POINT('Origin',(36.,7.75,5.));
#8379=CARTESIAN_POINT('Origin',(36.,7.2,5.));
#8380=CARTESIAN_POINT('',(35.85,7.9,5.77562877718661));
#8381=CARTESIAN_POINT('',(36.,7.75,5.79));
#8382=CARTESIAN_POINT('Origin',(36.,7.75,5.));
#8383=CARTESIAN_POINT('',(36.15,7.9,5.77562877718661));
#8384=CARTESIAN_POINT('Origin',(36.,7.9,5.));
#8385=CARTESIAN_POINT('Origin',(36.,7.75,5.));
#8386=CARTESIAN_POINT('Origin',(36.,7.2,5.));
#8387=CARTESIAN_POINT('',(36.45,7.3,4.35069267677008));
#8388=CARTESIAN_POINT('Origin',(36.,7.75,5.));
#8389=CARTESIAN_POINT('',(35.55,7.3,4.35069267677008));
#8390=CARTESIAN_POINT('Origin',(36.,7.75,5.));
#8391=CARTESIAN_POINT('Origin',(36.,7.3,5.));
#8392=CARTESIAN_POINT('Origin',(36.,7.2,5.));
#8393=CARTESIAN_POINT('',(35.55,7.3,5.64930732322992));
#8394=CARTESIAN_POINT('Origin',(36.,7.75,5.));
#8395=CARTESIAN_POINT('',(36.45,7.3,5.64930732322992));
#8396=CARTESIAN_POINT('Origin',(36.,7.75,5.));
#8397=CARTESIAN_POINT('Origin',(36.,7.3,5.));
#8398=CARTESIAN_POINT('Origin',(36.,7.9,5.));
#8399=CARTESIAN_POINT('',(-4.1,7.9,5.77562877718661));
#8400=CARTESIAN_POINT('Origin',(-4.1,7.75,5.));
#8401=CARTESIAN_POINT('',(0.,7.75,5.79));
#8402=CARTESIAN_POINT('',(-4.1,7.75,5.79));
#8403=CARTESIAN_POINT('',(-0.449999999999999,7.3,5.64930732322992));
#8404=CARTESIAN_POINT('Origin',(0.,7.75,5.));
#8405=CARTESIAN_POINT('',(-0.665807780068691,7.3,5.64930732322992));
#8406=CARTESIAN_POINT('',(-4.1,7.3,5.64930732322992));
#8407=CARTESIAN_POINT('',(-0.93,6.96,5.));
#8408=CARTESIAN_POINT('Ctrl Pts',(-0.665807780068692,7.3,5.64930732322992));
#8409=CARTESIAN_POINT('Ctrl Pts',(-0.692408622377835,7.26064211607598,5.62203048969952));
#8410=CARTESIAN_POINT('Ctrl Pts',(-0.718893727897336,7.22418930146339,5.59141801573814));
#8411=CARTESIAN_POINT('Ctrl Pts',(-0.793043306765111,7.12549314225287,5.49272185652762));
#8412=CARTESIAN_POINT('Ctrl Pts',(-0.842132255743763,7.06521916742952,5.40773913323974));
#8413=CARTESIAN_POINT('Ctrl Pts',(-0.910788192048256,6.98235868447187,5.21424953523639));
#8414=CARTESIAN_POINT('Ctrl Pts',(-0.93,6.96,5.10551936287513));
#8415=CARTESIAN_POINT('Ctrl Pts',(-0.93,6.96,5.));
#8416=CARTESIAN_POINT('',(-0.665807780068691,7.3,4.35069267677008));
#8417=CARTESIAN_POINT('Ctrl Pts',(-0.93,6.96,5.));
#8418=CARTESIAN_POINT('Ctrl Pts',(-0.93,6.96,4.89448063712487));
#8419=CARTESIAN_POINT('Ctrl Pts',(-0.910788192048256,6.98235868447187,4.78575046476361));
#8420=CARTESIAN_POINT('Ctrl Pts',(-0.842132255743762,7.06521916742952,4.59226086676026));
#8421=CARTESIAN_POINT('Ctrl Pts',(-0.793043306765111,7.12549314225287,4.50727814347238));
#8422=CARTESIAN_POINT('Ctrl Pts',(-0.718893727897336,7.22418930146339,4.40858198426186));
#8423=CARTESIAN_POINT('Ctrl Pts',(-0.692408622377835,7.26064211607598,4.37796951030048));
#8424=CARTESIAN_POINT('Ctrl Pts',(-0.665807780068692,7.3,4.35069267677008));
#8425=CARTESIAN_POINT('',(-0.449999999999999,7.3,4.35069267677008));
#8426=CARTESIAN_POINT('',(-4.1,7.3,4.35069267677008));
#8427=CARTESIAN_POINT('',(0.,7.75,4.21));
#8428=CARTESIAN_POINT('Origin',(0.,7.75,5.));
#8429=CARTESIAN_POINT('',(-0.15,7.9,4.22437122281339));
#8430=CARTESIAN_POINT('Origin',(0.,7.75,5.));
#8431=CARTESIAN_POINT('',(0.15,7.9,4.22437122281339));
#8432=CARTESIAN_POINT('',(-4.1,7.9,4.22437122281339));
#8433=CARTESIAN_POINT('Origin',(0.,7.75,5.));
#8434=CARTESIAN_POINT('',(0.449999999999999,7.3,4.35069267677008));
#8435=CARTESIAN_POINT('Origin',(0.,7.75,5.));
#8436=CARTESIAN_POINT('',(0.665807780068691,7.3,4.35069267677008));
#8437=CARTESIAN_POINT('',(-4.1,7.3,4.35069267677008));
#8438=CARTESIAN_POINT('',(0.665807780068691,7.3,5.64930732322992));
#8439=CARTESIAN_POINT('Ctrl Pts',(0.665807780068692,7.3,4.35069267677008));
#8440=CARTESIAN_POINT('Ctrl Pts',(0.692408622377835,7.26064211607598,4.37796951030048));
#8441=CARTESIAN_POINT('Ctrl Pts',(0.718893727897336,7.22418930146339,4.40858198426186));
#8442=CARTESIAN_POINT('Ctrl Pts',(0.793043306765111,7.12549314225287,4.50727814347238));
#8443=CARTESIAN_POINT('Ctrl Pts',(0.842132255743763,7.06521916742952,4.59226086676026));
#8444=CARTESIAN_POINT('Ctrl Pts',(0.910788192048256,6.98235868447187,4.78575046476361));
#8445=CARTESIAN_POINT('Ctrl Pts',(0.93,6.96,4.89448063712487));
#8446=CARTESIAN_POINT('Ctrl Pts',(0.93,6.96,5.10551936287513));
#8447=CARTESIAN_POINT('Ctrl Pts',(0.910788192048256,6.98235868447187,5.21424953523639));
#8448=CARTESIAN_POINT('Ctrl Pts',(0.842132255743762,7.06521916742952,5.40773913323974));
#8449=CARTESIAN_POINT('Ctrl Pts',(0.793043306765111,7.12549314225287,5.49272185652762));
#8450=CARTESIAN_POINT('Ctrl Pts',(0.718893727897336,7.22418930146339,5.59141801573814));
#8451=CARTESIAN_POINT('Ctrl Pts',(0.692408622377835,7.26064211607598,5.62203048969952));
#8452=CARTESIAN_POINT('Ctrl Pts',(0.665807780068692,7.3,5.64930732322992));
#8453=CARTESIAN_POINT('',(0.449999999999999,7.3,5.64930732322992));
#8454=CARTESIAN_POINT('',(-4.1,7.3,5.64930732322992));
#8455=CARTESIAN_POINT('Origin',(0.,7.75,5.));
#8456=CARTESIAN_POINT('',(12.,7.75,5.79));
#8457=CARTESIAN_POINT('',(-4.1,7.75,5.79));
#8458=CARTESIAN_POINT('',(11.55,7.3,5.64930732322992));
#8459=CARTESIAN_POINT('Origin',(12.,7.75,5.));
#8460=CARTESIAN_POINT('',(11.3341922199313,7.3,5.64930732322992));
#8461=CARTESIAN_POINT('',(-4.1,7.3,5.64930732322992));
#8462=CARTESIAN_POINT('',(11.07,6.96,5.));
#8463=CARTESIAN_POINT('Ctrl Pts',(11.3341922199313,7.3,5.64930732322992));
#8464=CARTESIAN_POINT('Ctrl Pts',(11.3075913776222,7.26064211607598,5.62203048969952));
#8465=CARTESIAN_POINT('Ctrl Pts',(11.2811062721027,7.22418930146339,5.59141801573814));
#8466=CARTESIAN_POINT('Ctrl Pts',(11.2069566932349,7.12549314225287,5.49272185652762));
#8467=CARTESIAN_POINT('Ctrl Pts',(11.1578677442562,7.06521916742952,5.40773913323974));
#8468=CARTESIAN_POINT('Ctrl Pts',(11.0892118079517,6.98235868447187,5.21424953523639));
#8469=CARTESIAN_POINT('Ctrl Pts',(11.07,6.96,5.10551936287513));
#8470=CARTESIAN_POINT('Ctrl Pts',(11.07,6.96,5.));
#8471=CARTESIAN_POINT('',(11.3341922199313,7.3,4.35069267677008));
#8472=CARTESIAN_POINT('Ctrl Pts',(11.07,6.96,5.));
#8473=CARTESIAN_POINT('Ctrl Pts',(11.07,6.96,4.89448063712487));
#8474=CARTESIAN_POINT('Ctrl Pts',(11.0892118079517,6.98235868447187,4.78575046476361));
#8475=CARTESIAN_POINT('Ctrl Pts',(11.1578677442562,7.06521916742952,4.59226086676026));
#8476=CARTESIAN_POINT('Ctrl Pts',(11.2069566932349,7.12549314225287,4.50727814347238));
#8477=CARTESIAN_POINT('Ctrl Pts',(11.2811062721027,7.22418930146339,4.40858198426186));
#8478=CARTESIAN_POINT('Ctrl Pts',(11.3075913776222,7.26064211607598,4.37796951030048));
#8479=CARTESIAN_POINT('Ctrl Pts',(11.3341922199313,7.3,4.35069267677008));
#8480=CARTESIAN_POINT('',(11.55,7.3,4.35069267677008));
#8481=CARTESIAN_POINT('',(-4.1,7.3,4.35069267677008));
#8482=CARTESIAN_POINT('',(12.,7.75,4.21));
#8483=CARTESIAN_POINT('Origin',(12.,7.75,5.));
#8484=CARTESIAN_POINT('',(11.85,7.9,4.22437122281339));
#8485=CARTESIAN_POINT('Origin',(12.,7.75,5.));
#8486=CARTESIAN_POINT('',(12.15,7.9,4.22437122281339));
#8487=CARTESIAN_POINT('',(-4.1,7.9,4.22437122281339));
#8488=CARTESIAN_POINT('Origin',(12.,7.75,5.));
#8489=CARTESIAN_POINT('',(12.45,7.3,4.35069267677008));
#8490=CARTESIAN_POINT('Origin',(12.,7.75,5.));
#8491=CARTESIAN_POINT('',(12.6658077800687,7.3,4.35069267677008));
#8492=CARTESIAN_POINT('',(-4.1,7.3,4.35069267677008));
#8493=CARTESIAN_POINT('',(12.6658077800687,7.3,5.64930732322992));
#8494=CARTESIAN_POINT('Ctrl Pts',(12.6658077800687,7.3,4.35069267677008));
#8495=CARTESIAN_POINT('Ctrl Pts',(12.6924086223778,7.26064211607598,4.37796951030047));
#8496=CARTESIAN_POINT('Ctrl Pts',(12.7188937278973,7.22418930146339,4.40858198426186));
#8497=CARTESIAN_POINT('Ctrl Pts',(12.7930433067651,7.12549314225287,4.50727814347238));
#8498=CARTESIAN_POINT('Ctrl Pts',(12.8421322557438,7.06521916742952,4.59226086676026));
#8499=CARTESIAN_POINT('Ctrl Pts',(12.9107881920483,6.98235868447187,4.78575046476361));
#8500=CARTESIAN_POINT('Ctrl Pts',(12.93,6.96,4.89448063712487));
#8501=CARTESIAN_POINT('Ctrl Pts',(12.93,6.96,5.10551936287513));
#8502=CARTESIAN_POINT('Ctrl Pts',(12.9107881920483,6.98235868447187,5.21424953523639));
#8503=CARTESIAN_POINT('Ctrl Pts',(12.8421322557438,7.06521916742952,5.40773913323974));
#8504=CARTESIAN_POINT('Ctrl Pts',(12.7930433067651,7.12549314225287,5.49272185652762));
#8505=CARTESIAN_POINT('Ctrl Pts',(12.7188937278973,7.22418930146339,5.59141801573814));
#8506=CARTESIAN_POINT('Ctrl Pts',(12.6924086223778,7.26064211607599,5.62203048969953));
#8507=CARTESIAN_POINT('Ctrl Pts',(12.6658077800687,7.3,5.64930732322992));
#8508=CARTESIAN_POINT('',(12.45,7.3,5.64930732322992));
#8509=CARTESIAN_POINT('',(-4.1,7.3,5.64930732322992));
#8510=CARTESIAN_POINT('Origin',(12.,7.75,5.));
#8511=CARTESIAN_POINT('',(24.,7.75,5.79));
#8512=CARTESIAN_POINT('',(-4.1,7.75,5.79));
#8513=CARTESIAN_POINT('',(23.55,7.3,5.64930732322992));
#8514=CARTESIAN_POINT('Origin',(24.,7.75,5.));
#8515=CARTESIAN_POINT('',(23.3341922199313,7.3,5.64930732322992));
#8516=CARTESIAN_POINT('',(-4.1,7.3,5.64930732322992));
#8517=CARTESIAN_POINT('',(23.07,6.96,5.));
#8518=CARTESIAN_POINT('Ctrl Pts',(23.3341922199313,7.3,5.64930732322992));
#8519=CARTESIAN_POINT('Ctrl Pts',(23.3075913776222,7.26064211607598,5.62203048969952));
#8520=CARTESIAN_POINT('Ctrl Pts',(23.2811062721027,7.2241893014634,5.59141801573814));
#8521=CARTESIAN_POINT('Ctrl Pts',(23.2069566932349,7.12549314225287,5.49272185652762));
#8522=CARTESIAN_POINT('Ctrl Pts',(23.1578677442562,7.06521916742952,5.40773913323974));
#8523=CARTESIAN_POINT('Ctrl Pts',(23.0892118079517,6.98235868447187,5.21424953523639));
#8524=CARTESIAN_POINT('Ctrl Pts',(23.07,6.96,5.10551936287513));
#8525=CARTESIAN_POINT('Ctrl Pts',(23.07,6.96,5.));
#8526=CARTESIAN_POINT('',(23.3341922199313,7.3,4.35069267677008));
#8527=CARTESIAN_POINT('Ctrl Pts',(23.07,6.96,5.));
#8528=CARTESIAN_POINT('Ctrl Pts',(23.07,6.96,4.89448063712487));
#8529=CARTESIAN_POINT('Ctrl Pts',(23.0892118079517,6.98235868447187,4.78575046476361));
#8530=CARTESIAN_POINT('Ctrl Pts',(23.1578677442562,7.06521916742952,4.59226086676026));
#8531=CARTESIAN_POINT('Ctrl Pts',(23.2069566932349,7.12549314225287,4.50727814347238));
#8532=CARTESIAN_POINT('Ctrl Pts',(23.2811062721027,7.2241893014634,4.40858198426186));
#8533=CARTESIAN_POINT('Ctrl Pts',(23.3075913776222,7.26064211607598,4.37796951030048));
#8534=CARTESIAN_POINT('Ctrl Pts',(23.3341922199313,7.3,4.35069267677008));
#8535=CARTESIAN_POINT('',(23.55,7.3,4.35069267677008));
#8536=CARTESIAN_POINT('',(-4.1,7.3,4.35069267677008));
#8537=CARTESIAN_POINT('',(24.,7.75,4.21));
#8538=CARTESIAN_POINT('Origin',(24.,7.75,5.));
#8539=CARTESIAN_POINT('',(23.85,7.9,4.22437122281339));
#8540=CARTESIAN_POINT('Origin',(24.,7.75,5.));
#8541=CARTESIAN_POINT('',(24.15,7.9,4.22437122281339));
#8542=CARTESIAN_POINT('',(-4.1,7.9,4.22437122281339));
#8543=CARTESIAN_POINT('Origin',(24.,7.75,5.));
#8544=CARTESIAN_POINT('',(24.45,7.3,4.35069267677008));
#8545=CARTESIAN_POINT('Origin',(24.,7.75,5.));
#8546=CARTESIAN_POINT('',(24.6658077800687,7.3,4.35069267677008));
#8547=CARTESIAN_POINT('',(-4.1,7.3,4.35069267677008));
#8548=CARTESIAN_POINT('',(24.6658077800687,7.3,5.64930732322992));
#8549=CARTESIAN_POINT('Ctrl Pts',(24.6658077800687,7.3,4.35069267677008));
#8550=CARTESIAN_POINT('Ctrl Pts',(24.6924086223778,7.26064211607598,4.37796951030048));
#8551=CARTESIAN_POINT('Ctrl Pts',(24.7188937278973,7.22418930146339,4.40858198426186));
#8552=CARTESIAN_POINT('Ctrl Pts',(24.7930433067651,7.12549314225287,4.50727814347238));
#8553=CARTESIAN_POINT('Ctrl Pts',(24.8421322557438,7.06521916742952,4.59226086676026));
#8554=CARTESIAN_POINT('Ctrl Pts',(24.9107881920483,6.98235868447187,4.78575046476361));
#8555=CARTESIAN_POINT('Ctrl Pts',(24.93,6.96,4.89448063712487));
#8556=CARTESIAN_POINT('Ctrl Pts',(24.93,6.96,5.10551936287513));
#8557=CARTESIAN_POINT('Ctrl Pts',(24.9107881920483,6.98235868447187,5.21424953523639));
#8558=CARTESIAN_POINT('Ctrl Pts',(24.8421322557438,7.06521916742952,5.40773913323974));
#8559=CARTESIAN_POINT('Ctrl Pts',(24.7930433067651,7.12549314225287,5.49272185652762));
#8560=CARTESIAN_POINT('Ctrl Pts',(24.7188937278973,7.22418930146339,5.59141801573814));
#8561=CARTESIAN_POINT('Ctrl Pts',(24.6924086223778,7.26064211607598,5.62203048969952));
#8562=CARTESIAN_POINT('Ctrl Pts',(24.6658077800687,7.3,5.64930732322992));
#8563=CARTESIAN_POINT('',(24.45,7.3,5.64930732322992));
#8564=CARTESIAN_POINT('',(-4.1,7.3,5.64930732322992));
#8565=CARTESIAN_POINT('Origin',(24.,7.75,5.));
#8566=CARTESIAN_POINT('',(-4.1,7.75,5.79));
#8567=CARTESIAN_POINT('',(35.3341922199313,7.3,5.64930732322992));
#8568=CARTESIAN_POINT('',(-4.1,7.3,5.64930732322992));
#8569=CARTESIAN_POINT('',(35.07,6.96,5.));
#8570=CARTESIAN_POINT('Ctrl Pts',(35.3341922199313,7.3,5.64930732322992));
#8571=CARTESIAN_POINT('Ctrl Pts',(35.3075913776222,7.26064211607598,5.62203048969952));
#8572=CARTESIAN_POINT('Ctrl Pts',(35.2811062721027,7.2241893014634,5.59141801573814));
#8573=CARTESIAN_POINT('Ctrl Pts',(35.2069566932349,7.12549314225287,5.49272185652762));
#8574=CARTESIAN_POINT('Ctrl Pts',(35.1578677442562,7.06521916742952,5.40773913323974));
#8575=CARTESIAN_POINT('Ctrl Pts',(35.0892118079517,6.98235868447187,5.21424953523639));
#8576=CARTESIAN_POINT('Ctrl Pts',(35.07,6.96,5.10551936287513));
#8577=CARTESIAN_POINT('Ctrl Pts',(35.07,6.96,5.));
#8578=CARTESIAN_POINT('',(35.3341922199313,7.3,4.35069267677008));
#8579=CARTESIAN_POINT('Ctrl Pts',(35.07,6.96,5.));
#8580=CARTESIAN_POINT('Ctrl Pts',(35.07,6.96,4.89448063712487));
#8581=CARTESIAN_POINT('Ctrl Pts',(35.0892118079517,6.98235868447187,4.78575046476361));
#8582=CARTESIAN_POINT('Ctrl Pts',(35.1578677442562,7.06521916742952,4.59226086676026));
#8583=CARTESIAN_POINT('Ctrl Pts',(35.2069566932349,7.12549314225287,4.50727814347238));
#8584=CARTESIAN_POINT('Ctrl Pts',(35.2811062721027,7.22418930146339,4.40858198426186));
#8585=CARTESIAN_POINT('Ctrl Pts',(35.3075913776222,7.26064211607598,4.37796951030048));
#8586=CARTESIAN_POINT('Ctrl Pts',(35.3341922199313,7.3,4.35069267677008));
#8587=CARTESIAN_POINT('',(-4.1,7.3,4.35069267677008));
#8588=CARTESIAN_POINT('',(36.6658077800687,7.3,4.35069267677008));
#8589=CARTESIAN_POINT('',(-4.1,7.3,4.35069267677008));
#8590=CARTESIAN_POINT('',(36.6658077800687,7.3,5.64930732322992));
#8591=CARTESIAN_POINT('Ctrl Pts',(36.6658077800687,7.3,4.35069267677008));
#8592=CARTESIAN_POINT('Ctrl Pts',(36.6924086223778,7.26064211607598,4.37796951030048));
#8593=CARTESIAN_POINT('Ctrl Pts',(36.7188937278973,7.22418930146339,4.40858198426186));
#8594=CARTESIAN_POINT('Ctrl Pts',(36.7930433067651,7.12549314225287,4.50727814347238));
#8595=CARTESIAN_POINT('Ctrl Pts',(36.8421322557438,7.06521916742952,4.59226086676026));
#8596=CARTESIAN_POINT('Ctrl Pts',(36.9107881920483,6.98235868447187,4.78575046476361));
#8597=CARTESIAN_POINT('Ctrl Pts',(36.93,6.96,4.89448063712487));
#8598=CARTESIAN_POINT('Ctrl Pts',(36.93,6.96,5.10551936287513));
#8599=CARTESIAN_POINT('Ctrl Pts',(36.9107881920483,6.98235868447187,5.21424953523639));
#8600=CARTESIAN_POINT('Ctrl Pts',(36.8421322557438,7.06521916742952,5.40773913323974));
#8601=CARTESIAN_POINT('Ctrl Pts',(36.7930433067651,7.12549314225287,5.49272185652762));
#8602=CARTESIAN_POINT('Ctrl Pts',(36.7188937278973,7.22418930146339,5.59141801573814));
#8603=CARTESIAN_POINT('Ctrl Pts',(36.6924086223778,7.26064211607598,5.62203048969952));
#8604=CARTESIAN_POINT('Ctrl Pts',(36.6658077800687,7.3,5.64930732322992));
#8605=CARTESIAN_POINT('',(-4.1,7.3,5.64930732322992));
#8606=CARTESIAN_POINT('',(-4.1,7.75,5.79));
#8607=CARTESIAN_POINT('',(24.15,7.9,5.77562877718661));
#8608=CARTESIAN_POINT('Origin',(24.,7.75,5.));
#8609=CARTESIAN_POINT('',(23.85,7.9,5.77562877718661));
#8610=CARTESIAN_POINT('',(-4.1,7.9,5.77562877718661));
#8611=CARTESIAN_POINT('Origin',(24.,7.75,5.));
#8612=CARTESIAN_POINT('',(12.15,7.9,5.77562877718661));
#8613=CARTESIAN_POINT('Origin',(12.,7.75,5.));
#8614=CARTESIAN_POINT('',(11.85,7.9,5.77562877718661));
#8615=CARTESIAN_POINT('',(-4.1,7.9,5.77562877718661));
#8616=CARTESIAN_POINT('Origin',(12.,7.75,5.));
#8617=CARTESIAN_POINT('',(0.15,7.9,5.77562877718661));
#8618=CARTESIAN_POINT('Origin',(0.,7.75,5.));
#8619=CARTESIAN_POINT('',(-0.15,7.9,5.77562877718661));
#8620=CARTESIAN_POINT('',(-4.1,7.9,5.77562877718661));
#8621=CARTESIAN_POINT('Origin',(0.,7.75,5.));
#8622=CARTESIAN_POINT('Origin',(36.,7.3,5.));
#8623=CARTESIAN_POINT('Origin',(36.,7.3,5.));
#8624=CARTESIAN_POINT('Origin',(36.,5.9,5.));
#8625=CARTESIAN_POINT('',(35.07,6.,5.));
#8626=CARTESIAN_POINT('Origin',(36.,6.,5.));
#8627=CARTESIAN_POINT('',(35.07,5.9,5.));
#8628=CARTESIAN_POINT('Origin',(36.,7.3,5.));
#8629=CARTESIAN_POINT('Origin',(36.,7.3,5.));
#8630=CARTESIAN_POINT('Origin',(24.,7.9,5.));
#8631=CARTESIAN_POINT('Origin',(24.,7.9,5.));
#8632=CARTESIAN_POINT('Origin',(24.,7.2,5.));
#8633=CARTESIAN_POINT('Origin',(24.,7.2,5.));
#8634=CARTESIAN_POINT('Origin',(24.,7.9,5.));
#8635=CARTESIAN_POINT('Origin',(24.,7.2,5.));
#8636=CARTESIAN_POINT('Origin',(24.,7.3,5.));
#8637=CARTESIAN_POINT('Origin',(24.,7.2,5.));
#8638=CARTESIAN_POINT('Origin',(24.,7.3,5.));
#8639=CARTESIAN_POINT('Origin',(24.,7.9,5.));
#8640=CARTESIAN_POINT('Origin',(24.,7.3,5.));
#8641=CARTESIAN_POINT('Origin',(24.,7.3,5.));
#8642=CARTESIAN_POINT('Origin',(24.,5.9,5.));
#8643=CARTESIAN_POINT('',(23.07,6.,5.));
#8644=CARTESIAN_POINT('Origin',(24.,6.,5.));
#8645=CARTESIAN_POINT('',(23.07,5.9,5.));
#8646=CARTESIAN_POINT('Origin',(24.,7.3,5.));
#8647=CARTESIAN_POINT('Origin',(24.,7.3,5.));
#8648=CARTESIAN_POINT('Origin',(12.,7.9,5.));
#8649=CARTESIAN_POINT('Origin',(12.,7.9,5.));
#8650=CARTESIAN_POINT('Origin',(12.,7.2,5.));
#8651=CARTESIAN_POINT('Origin',(12.,7.2,5.));
#8652=CARTESIAN_POINT('Origin',(12.,7.9,5.));
#8653=CARTESIAN_POINT('Origin',(12.,7.2,5.));
#8654=CARTESIAN_POINT('Origin',(12.,7.3,5.));
#8655=CARTESIAN_POINT('Origin',(12.,7.2,5.));
#8656=CARTESIAN_POINT('Origin',(12.,7.3,5.));
#8657=CARTESIAN_POINT('Origin',(12.,7.9,5.));
#8658=CARTESIAN_POINT('Origin',(12.,7.3,5.));
#8659=CARTESIAN_POINT('Origin',(12.,7.3,5.));
#8660=CARTESIAN_POINT('Origin',(12.,5.9,5.));
#8661=CARTESIAN_POINT('',(11.07,6.,5.));
#8662=CARTESIAN_POINT('Origin',(12.,6.,5.));
#8663=CARTESIAN_POINT('',(11.07,5.9,5.));
#8664=CARTESIAN_POINT('Origin',(12.,7.3,5.));
#8665=CARTESIAN_POINT('Origin',(12.,7.3,5.));
#8666=CARTESIAN_POINT('Origin',(0.,7.9,5.));
#8667=CARTESIAN_POINT('Origin',(0.,7.9,5.));
#8668=CARTESIAN_POINT('Origin',(0.,7.2,5.));
#8669=CARTESIAN_POINT('Origin',(0.,7.2,5.));
#8670=CARTESIAN_POINT('Origin',(0.,7.9,5.));
#8671=CARTESIAN_POINT('Origin',(0.,7.2,5.));
#8672=CARTESIAN_POINT('Origin',(0.,7.3,5.));
#8673=CARTESIAN_POINT('Origin',(0.,7.2,5.));
#8674=CARTESIAN_POINT('Origin',(0.,7.3,5.));
#8675=CARTESIAN_POINT('Origin',(0.,7.9,5.));
#8676=CARTESIAN_POINT('Origin',(0.,7.3,5.));
#8677=CARTESIAN_POINT('Origin',(0.,7.3,5.));
#8678=CARTESIAN_POINT('Origin',(0.,5.9,5.));
#8679=CARTESIAN_POINT('',(-0.93,6.,5.));
#8680=CARTESIAN_POINT('Origin',(0.,6.,5.));
#8681=CARTESIAN_POINT('',(-0.93,5.9,5.));
#8682=CARTESIAN_POINT('Origin',(0.,7.3,5.));
#8683=CARTESIAN_POINT('Origin',(0.,7.3,5.));
#8684=CARTESIAN_POINT('Origin',(40.,9.5,3.5));
#8685=CARTESIAN_POINT('',(40.,9.5,3.5));
#8686=CARTESIAN_POINT('',(-4.,9.5,3.5));
#8687=CARTESIAN_POINT('',(40.,9.5,3.5));
#8688=CARTESIAN_POINT('',(-4.,9.5,6.5));
#8689=CARTESIAN_POINT('',(-4.,9.5,3.5));
#8690=CARTESIAN_POINT('',(40.,9.5,6.5));
#8691=CARTESIAN_POINT('',(40.,9.5,6.5));
#8692=CARTESIAN_POINT('',(40.,9.5,3.5));
#8693=CARTESIAN_POINT('Origin',(40.,6.,3.5));
#8694=CARTESIAN_POINT('',(40.,6.,3.5));
#8695=CARTESIAN_POINT('',(40.,6.,3.5));
#8696=CARTESIAN_POINT('',(40.,6.,6.5));
#8697=CARTESIAN_POINT('',(40.,6.,6.5));
#8698=CARTESIAN_POINT('',(40.,6.,3.5));
#8699=CARTESIAN_POINT('Origin',(-4.,6.,3.5));
#8700=CARTESIAN_POINT('',(-4.,6.,3.5));
#8701=CARTESIAN_POINT('',(-4.,6.,3.5));
#8702=CARTESIAN_POINT('',(-4.,6.,6.5));
#8703=CARTESIAN_POINT('',(-4.,6.,6.5));
#8704=CARTESIAN_POINT('',(-4.,6.,3.5));
#8705=CARTESIAN_POINT('Origin',(-4.,9.5,3.5));
#8706=CARTESIAN_POINT('',(-4.,9.5,3.5));
#8707=CARTESIAN_POINT('',(-4.,9.5,6.5));
#8708=CARTESIAN_POINT('Origin',(18.,7.75,6.5));
#8709=CARTESIAN_POINT('Origin',(18.,7.75,3.5));
#8710=CARTESIAN_POINT('',(0.,0.,0.));
#8711=CARTESIAN_POINT('Origin',(-4.,7.75,5.));
#8712=CARTESIAN_POINT('',(-4.,8.44282032302755,3.8));
#8713=CARTESIAN_POINT('',(-4.,9.1356406460551,5.));
#8714=CARTESIAN_POINT('',(-4.,8.44282032302755,3.8));
#8715=CARTESIAN_POINT('',(-4.,8.44282032302755,6.2));
#8716=CARTESIAN_POINT('',(-4.,9.1356406460551,5.));
#8717=CARTESIAN_POINT('',(-4.,7.05717967697245,6.2));
#8718=CARTESIAN_POINT('',(-4.,8.44282032302755,6.2));
#8719=CARTESIAN_POINT('',(-4.,6.3643593539449,5.));
#8720=CARTESIAN_POINT('',(-4.,7.05717967697245,6.2));
#8721=CARTESIAN_POINT('',(-4.,7.05717967697245,3.8));
#8722=CARTESIAN_POINT('',(-4.,6.3643593539449,5.));
#8723=CARTESIAN_POINT('',(-4.,7.05717967697245,3.8));
#8724=CARTESIAN_POINT('',(-4.,7.75,5.93));
#8725=CARTESIAN_POINT('Origin',(-4.,7.75,5.));
#8726=CARTESIAN_POINT('Origin',(-4.6,7.05717967697245,3.8));
#8727=CARTESIAN_POINT('',(-4.6,7.05717967697245,3.8));
#8728=CARTESIAN_POINT('',(-4.6,8.44282032302755,3.8));
#8729=CARTESIAN_POINT('',(-4.6,7.05717967697245,3.8));
#8730=CARTESIAN_POINT('',(-4.6,8.44282032302755,3.8));
#8731=CARTESIAN_POINT('',(-4.6,7.05717967697245,3.8));
#8732=CARTESIAN_POINT('Origin',(-4.6,6.3643593539449,5.));
#8733=CARTESIAN_POINT('',(-4.6,6.3643593539449,5.));
#8734=CARTESIAN_POINT('',(-4.6,6.3643593539449,5.));
#8735=CARTESIAN_POINT('',(-4.6,6.3643593539449,5.));
#8736=CARTESIAN_POINT('Origin',(-4.6,7.05717967697245,6.2));
#8737=CARTESIAN_POINT('',(-4.6,7.05717967697245,6.2));
#8738=CARTESIAN_POINT('',(-4.6,7.05717967697245,6.2));
#8739=CARTESIAN_POINT('',(-4.6,7.05717967697245,6.2));
#8740=CARTESIAN_POINT('Origin',(-4.6,8.44282032302755,6.2));
#8741=CARTESIAN_POINT('',(-4.6,8.44282032302755,6.2));
#8742=CARTESIAN_POINT('',(-4.6,8.44282032302755,6.2));
#8743=CARTESIAN_POINT('',(-4.6,8.44282032302755,6.2));
#8744=CARTESIAN_POINT('Origin',(-4.6,9.1356406460551,5.));
#8745=CARTESIAN_POINT('',(-4.6,9.1356406460551,5.));
#8746=CARTESIAN_POINT('',(-4.6,9.1356406460551,5.));
#8747=CARTESIAN_POINT('',(-4.6,9.1356406460551,5.));
#8748=CARTESIAN_POINT('Origin',(-4.6,8.44282032302755,3.8));
#8749=CARTESIAN_POINT('',(-4.6,8.44282032302755,3.8));
#8750=CARTESIAN_POINT('Origin',(-4.6,7.75,5.));
#8751=CARTESIAN_POINT('Origin',(-4.,7.75,5.));
#8752=CARTESIAN_POINT('',(-2.7,7.75,5.93));
#8753=CARTESIAN_POINT('Origin',(-2.7,7.75,5.));
#8754=CARTESIAN_POINT('',(-4.,7.75,5.93));
#8755=CARTESIAN_POINT('Origin',(-2.7,7.75,5.));
#8756=CARTESIAN_POINT('',(0.,0.,0.));
#8757=CARTESIAN_POINT('Origin',(-1.1,10.,0.8));
#8758=CARTESIAN_POINT('',(-1.65,10.,0.8));
#8759=CARTESIAN_POINT('Origin',(-1.1,10.,0.8));
#8760=CARTESIAN_POINT('',(-1.65,10.,3.5));
#8761=CARTESIAN_POINT('',(-1.65,10.,0.8));
#8762=CARTESIAN_POINT('Origin',(-1.1,10.,3.5));
#8763=CARTESIAN_POINT('Origin',(-1.1,10.,0.8));
#8764=CARTESIAN_POINT('',(-1.43,10.,0.8));
#8765=CARTESIAN_POINT('Origin',(-1.1,10.,0.8));
#8766=CARTESIAN_POINT('Origin',(-1.1,10.,-0.1));
#8767=CARTESIAN_POINT('',(-1.43,10.,0.));
#8768=CARTESIAN_POINT('Origin',(-1.1,10.,0.));
#8769=CARTESIAN_POINT('',(-1.43,10.,-0.1));
#8770=CARTESIAN_POINT('Origin',(-3.9,10.,0.8));
#8771=CARTESIAN_POINT('',(-4.45,10.,0.8));
#8772=CARTESIAN_POINT('Origin',(-3.9,10.,0.8));
#8773=CARTESIAN_POINT('',(-4.45,10.,3.5));
#8774=CARTESIAN_POINT('',(-4.45,10.,0.8));
#8775=CARTESIAN_POINT('Origin',(-3.9,10.,3.5));
#8776=CARTESIAN_POINT('Origin',(-3.9,10.,0.8));
#8777=CARTESIAN_POINT('',(-4.23,10.,0.8));
#8778=CARTESIAN_POINT('Origin',(-3.9,10.,0.8));
#8779=CARTESIAN_POINT('Origin',(-3.9,10.,-0.1));
#8780=CARTESIAN_POINT('',(-4.23,10.,0.));
#8781=CARTESIAN_POINT('Origin',(-3.9,10.,0.));
#8782=CARTESIAN_POINT('',(-4.23,10.,-0.1));
#8783=CARTESIAN_POINT('Origin',(-2.5,9.,-0.1));
#8784=CARTESIAN_POINT('',(-3.1,9.,0.));
#8785=CARTESIAN_POINT('Origin',(-2.5,9.,0.));
#8786=CARTESIAN_POINT('',(-3.1,9.,2.1));
#8787=CARTESIAN_POINT('',(-3.1,9.,-0.1));
#8788=CARTESIAN_POINT('Origin',(-2.5,9.,2.1));
#8789=CARTESIAN_POINT('Origin',(-2.5,9.,2.1));
#8790=CARTESIAN_POINT('',(-2.83,9.,2.1));
#8791=CARTESIAN_POINT('Origin',(-2.5,9.,2.1));
#8792=CARTESIAN_POINT('Origin',(-2.5,9.,-0.1));
#8793=CARTESIAN_POINT('',(-2.83,9.,3.5));
#8794=CARTESIAN_POINT('',(-2.83,9.,-0.1));
#8795=CARTESIAN_POINT('Origin',(-2.5,9.,3.5));
#8796=CARTESIAN_POINT('Origin',(-0.5,11.,0.));
#8797=CARTESIAN_POINT('',(-0.5,11.,0.));
#8798=CARTESIAN_POINT('',(-4.5,11.,0.));
#8799=CARTESIAN_POINT('',(-0.5,11.,0.));
#8800=CARTESIAN_POINT('',(-4.5,11.,3.5));
#8801=CARTESIAN_POINT('',(-4.5,11.,0.));
#8802=CARTESIAN_POINT('',(-0.5,11.,3.5));
#8803=CARTESIAN_POINT('',(-0.5,11.,3.5));
#8804=CARTESIAN_POINT('',(-0.5,11.,0.));
#8805=CARTESIAN_POINT('Origin',(-0.5,8.,0.));
#8806=CARTESIAN_POINT('',(-0.5,8.,0.));
#8807=CARTESIAN_POINT('',(-0.5,8.,0.));
#8808=CARTESIAN_POINT('',(-0.5,8.,3.5));
#8809=CARTESIAN_POINT('',(-0.5,8.,3.5));
#8810=CARTESIAN_POINT('',(-0.5,8.,0.));
#8811=CARTESIAN_POINT('Origin',(-4.5,8.,0.));
#8812=CARTESIAN_POINT('',(-4.5,8.,0.));
#8813=CARTESIAN_POINT('',(-4.5,8.,0.));
#8814=CARTESIAN_POINT('',(-4.5,8.,3.5));
#8815=CARTESIAN_POINT('',(-4.5,8.,3.5));
#8816=CARTESIAN_POINT('',(-4.5,8.,0.));
#8817=CARTESIAN_POINT('Origin',(-4.5,11.,0.));
#8818=CARTESIAN_POINT('',(-4.5,11.,0.));
#8819=CARTESIAN_POINT('',(-4.5,11.,3.5));
#8820=CARTESIAN_POINT('Origin',(-2.5,9.5,3.5));
#8821=CARTESIAN_POINT('Origin',(-2.5,9.5,0.));
#8822=CARTESIAN_POINT('',(0.,0.,0.));
#8823=CARTESIAN_POINT('Origin',(39.9,10.,0.8));
#8824=CARTESIAN_POINT('',(39.35,10.,0.8));
#8825=CARTESIAN_POINT('Origin',(39.9,10.,0.8));
#8826=CARTESIAN_POINT('',(39.35,10.,3.5));
#8827=CARTESIAN_POINT('',(39.35,10.,0.8));
#8828=CARTESIAN_POINT('Origin',(39.9,10.,3.5));
#8829=CARTESIAN_POINT('Origin',(39.9,10.,0.8));
#8830=CARTESIAN_POINT('',(39.57,10.,0.8));
#8831=CARTESIAN_POINT('Origin',(39.9,10.,0.8));
#8832=CARTESIAN_POINT('Origin',(39.9,10.,-0.1));
#8833=CARTESIAN_POINT('',(39.57,10.,0.));
#8834=CARTESIAN_POINT('Origin',(39.9,10.,0.));
#8835=CARTESIAN_POINT('',(39.57,10.,-0.1));
#8836=CARTESIAN_POINT('Origin',(37.1,10.,0.8));
#8837=CARTESIAN_POINT('',(36.55,10.,0.8));
#8838=CARTESIAN_POINT('Origin',(37.1,10.,0.8));
#8839=CARTESIAN_POINT('',(36.55,10.,3.5));
#8840=CARTESIAN_POINT('',(36.55,10.,0.8));
#8841=CARTESIAN_POINT('Origin',(37.1,10.,3.5));
#8842=CARTESIAN_POINT('Origin',(37.1,10.,0.8));
#8843=CARTESIAN_POINT('',(36.77,10.,0.8));
#8844=CARTESIAN_POINT('Origin',(37.1,10.,0.8));
#8845=CARTESIAN_POINT('Origin',(37.1,10.,-0.1));
#8846=CARTESIAN_POINT('',(36.77,10.,0.));
#8847=CARTESIAN_POINT('Origin',(37.1,10.,0.));
#8848=CARTESIAN_POINT('',(36.77,10.,-0.1));
#8849=CARTESIAN_POINT('Origin',(38.5,9.,-0.1));
#8850=CARTESIAN_POINT('',(37.9,9.,0.));
#8851=CARTESIAN_POINT('Origin',(38.5,9.,0.));
#8852=CARTESIAN_POINT('',(37.9,9.,2.1));
#8853=CARTESIAN_POINT('',(37.9,9.,-0.1));
#8854=CARTESIAN_POINT('Origin',(38.5,9.,2.1));
#8855=CARTESIAN_POINT('Origin',(38.5,9.,2.1));
#8856=CARTESIAN_POINT('',(38.17,9.,2.1));
#8857=CARTESIAN_POINT('Origin',(38.5,9.,2.1));
#8858=CARTESIAN_POINT('Origin',(38.5,9.,-0.1));
#8859=CARTESIAN_POINT('',(38.17,9.,3.5));
#8860=CARTESIAN_POINT('',(38.17,9.,-0.1));
#8861=CARTESIAN_POINT('Origin',(38.5,9.,3.5));
#8862=CARTESIAN_POINT('Origin',(40.5,11.,0.));
#8863=CARTESIAN_POINT('',(40.5,11.,0.));
#8864=CARTESIAN_POINT('',(36.5,11.,0.));
#8865=CARTESIAN_POINT('',(40.5,11.,0.));
#8866=CARTESIAN_POINT('',(36.5,11.,3.5));
#8867=CARTESIAN_POINT('',(36.5,11.,0.));
#8868=CARTESIAN_POINT('',(40.5,11.,3.5));
#8869=CARTESIAN_POINT('',(40.5,11.,3.5));
#8870=CARTESIAN_POINT('',(40.5,11.,0.));
#8871=CARTESIAN_POINT('Origin',(40.5,8.,0.));
#8872=CARTESIAN_POINT('',(40.5,8.,0.));
#8873=CARTESIAN_POINT('',(40.5,8.,0.));
#8874=CARTESIAN_POINT('',(40.5,8.,3.5));
#8875=CARTESIAN_POINT('',(40.5,8.,3.5));
#8876=CARTESIAN_POINT('',(40.5,8.,0.));
#8877=CARTESIAN_POINT('Origin',(36.5,8.,0.));
#8878=CARTESIAN_POINT('',(36.5,8.,0.));
#8879=CARTESIAN_POINT('',(36.5,8.,0.));
#8880=CARTESIAN_POINT('',(36.5,8.,3.5));
#8881=CARTESIAN_POINT('',(36.5,8.,3.5));
#8882=CARTESIAN_POINT('',(36.5,8.,0.));
#8883=CARTESIAN_POINT('Origin',(36.5,11.,0.));
#8884=CARTESIAN_POINT('',(36.5,11.,0.));
#8885=CARTESIAN_POINT('',(36.5,11.,3.5));
#8886=CARTESIAN_POINT('Origin',(38.5,9.5,3.5));
#8887=CARTESIAN_POINT('Origin',(38.5,9.5,0.));
#8888=CARTESIAN_POINT('',(0.,0.,0.));
#8889=CARTESIAN_POINT('Origin',(0.,-1.445,0.));
#8890=CARTESIAN_POINT('',(-0.2942,-2.9458,3.60291088309151E-17));
#8891=CARTESIAN_POINT('Origin',(0.,-2.9458,0.));
#8892=CARTESIAN_POINT('',(-0.2942,0.,-3.60291088309151E-17));
#8893=CARTESIAN_POINT('',(-0.2942,-1.445,-3.60291088309151E-17));
#8894=CARTESIAN_POINT('Origin',(0.,0.,0.));
#8895=CARTESIAN_POINT('Origin',(0.,-2.97,0.));
#8896=CARTESIAN_POINT('',(-0.24,-3.,-2.93915231795365E-17));
#8897=CARTESIAN_POINT('Origin',(0.,-3.,0.));
#8898=CARTESIAN_POINT('',(-0.27,-2.97,-3.30654635769785E-17));
#8899=CARTESIAN_POINT('Origin',(0.,-3.,0.));
#8900=CARTESIAN_POINT('Origin',(0.,0.341586508806388,0.));
#8901=CARTESIAN_POINT('',(-0.475,0.4,-5.81707229594993E-17));
#8902=CARTESIAN_POINT('Origin',(0.,0.4,0.));
#8903=CARTESIAN_POINT('',(-0.577350269189626,0.340908044531739,-7.07050159149938E-17));
#8904=CARTESIAN_POINT('',(-0.576175134594813,0.341586508806388,-7.05611034329833E-17));
#8905=CARTESIAN_POINT('',(-0.288675134594813,0.340908044531739,0.5));
#8906=CARTESIAN_POINT('Ctrl Pts',(-0.288675134594813,0.340908044531739,
0.5));
#8907=CARTESIAN_POINT('Ctrl Pts',(-0.433012701893303,0.424241377863696,
0.249999999998124));
#8908=CARTESIAN_POINT('Ctrl Pts',(-0.577350269189626,0.340908044531739,
-7.07050159149938E-17));
#8909=CARTESIAN_POINT('',(0.288675134594813,0.340908044531739,0.5));
#8910=CARTESIAN_POINT('Ctrl Pts',(0.288675134594813,0.340908044531739,0.5));
#8911=CARTESIAN_POINT('Ctrl Pts',(-2.16648921025353E-12,0.424241377863696,
0.5));
#8912=CARTESIAN_POINT('Ctrl Pts',(-0.288675134594813,0.340908044531739,
0.5));
#8913=CARTESIAN_POINT('',(0.577350269189626,0.340908044531739,0.));
#8914=CARTESIAN_POINT('Ctrl Pts',(0.577350269189626,0.340908044531739,0.));
#8915=CARTESIAN_POINT('Ctrl Pts',(0.433012701891136,0.424241377863697,0.250000000001876));
#8916=CARTESIAN_POINT('Ctrl Pts',(0.288675134594813,0.340908044531739,0.5));
#8917=CARTESIAN_POINT('',(0.288675134594813,0.340908044531739,-0.5));
#8918=CARTESIAN_POINT('Ctrl Pts',(0.288675134594813,0.340908044531739,-0.5));
#8919=CARTESIAN_POINT('Ctrl Pts',(0.433012701893303,0.424241377863696,-0.249999999998124));
#8920=CARTESIAN_POINT('Ctrl Pts',(0.577350269189626,0.340908044531739,0.));
#8921=CARTESIAN_POINT('',(-0.288675134594813,0.340908044531739,-0.5));
#8922=CARTESIAN_POINT('Ctrl Pts',(-0.288675134594813,0.340908044531739,
-0.5));
#8923=CARTESIAN_POINT('Ctrl Pts',(2.16660023255599E-12,0.424241377863696,
-0.5));
#8924=CARTESIAN_POINT('Ctrl Pts',(0.288675134594813,0.340908044531739,-0.5));
#8925=CARTESIAN_POINT('Ctrl Pts',(-0.577350269189626,0.340908044531739,
-7.07050159149938E-17));
#8926=CARTESIAN_POINT('Ctrl Pts',(-0.433012701891136,0.424241377863697,
-0.250000000001876));
#8927=CARTESIAN_POINT('Ctrl Pts',(-0.288675134594813,0.340908044531739,
-0.5));
#8928=CARTESIAN_POINT('Origin',(0.288675134594813,0.,-0.5));
#8929=CARTESIAN_POINT('',(0.288675134594813,0.,-0.5));
#8930=CARTESIAN_POINT('',(0.288675134594813,0.,-0.5));
#8931=CARTESIAN_POINT('',(-0.288675134594813,0.,-0.5));
#8932=CARTESIAN_POINT('',(0.288675134594813,0.,-0.5));
#8933=CARTESIAN_POINT('',(-0.288675134594813,0.,-0.5));
#8934=CARTESIAN_POINT('Origin',(0.577350269189626,0.,0.));
#8935=CARTESIAN_POINT('',(0.577350269189626,0.,0.));
#8936=CARTESIAN_POINT('',(0.577350269189626,0.,0.));
#8937=CARTESIAN_POINT('',(0.577350269189626,0.,0.));
#8938=CARTESIAN_POINT('Origin',(0.288675134594813,0.,0.5));
#8939=CARTESIAN_POINT('',(0.288675134594813,0.,0.5));
#8940=CARTESIAN_POINT('',(0.288675134594813,0.,0.5));
#8941=CARTESIAN_POINT('',(0.288675134594813,0.,0.5));
#8942=CARTESIAN_POINT('Origin',(-0.288675134594813,0.,0.5));
#8943=CARTESIAN_POINT('',(-0.288675134594813,0.,0.5));
#8944=CARTESIAN_POINT('',(-0.288675134594813,0.,0.5));
#8945=CARTESIAN_POINT('',(-0.288675134594813,0.,0.5));
#8946=CARTESIAN_POINT('Origin',(-0.577350269189626,0.,-7.07050159149938E-17));
#8947=CARTESIAN_POINT('',(-0.577350269189626,0.,-7.07050159149938E-17));
#8948=CARTESIAN_POINT('',(-0.577350269189626,0.,-7.07050159149938E-17));
#8949=CARTESIAN_POINT('',(-0.577350269189626,0.,-7.07050159149938E-17));
#8950=CARTESIAN_POINT('Origin',(-0.288675134594813,0.,-0.5));
#8951=CARTESIAN_POINT('',(-0.288675134594813,0.,-0.5));
#8952=CARTESIAN_POINT('Origin',(0.,0.4,0.));
#8953=CARTESIAN_POINT('Origin',(0.,0.,0.));
#8954=CARTESIAN_POINT('',(0.,0.,0.));
#8955=CARTESIAN_POINT('',(0.,0.,0.));
#8956=CARTESIAN_POINT('Origin',(-1.3,-1.,6.8));
#8957=CARTESIAN_POINT('',(-1.465,-1.,6.8));
#8958=CARTESIAN_POINT('Origin',(-1.3,-1.,6.8));
#8959=CARTESIAN_POINT('',(-1.465,-1.,7.5));
#8960=CARTESIAN_POINT('',(-1.465,-1.,6.8));
#8961=CARTESIAN_POINT('Origin',(-1.3,-1.,7.5));
#8962=CARTESIAN_POINT('Origin',(-1.3,-1.,6.8));
#8963=CARTESIAN_POINT('Origin',(1.3,-1.,6.8));
#8964=CARTESIAN_POINT('',(1.135,-1.,6.8));
#8965=CARTESIAN_POINT('Origin',(1.3,-1.,6.8));
#8966=CARTESIAN_POINT('',(1.135,-1.,7.5));
#8967=CARTESIAN_POINT('',(1.135,-1.,6.8));
#8968=CARTESIAN_POINT('Origin',(1.3,-1.,7.5));
#8969=CARTESIAN_POINT('Origin',(1.3,-1.,6.8));
#8970=CARTESIAN_POINT('Origin',(1.9,-3.1,3.1));
#8971=CARTESIAN_POINT('',(1.625,-3.,3.1));
#8972=CARTESIAN_POINT('Origin',(1.9,-3.,3.1));
#8973=CARTESIAN_POINT('',(1.625,-0.0249999999999999,3.1));
#8974=CARTESIAN_POINT('',(1.625,-3.1,3.1));
#8975=CARTESIAN_POINT('Origin',(1.9,-0.0249999999999999,3.1));
#8976=CARTESIAN_POINT('Origin',(-1.9,-3.1,6.9));
#8977=CARTESIAN_POINT('',(-2.175,-3.,6.9));
#8978=CARTESIAN_POINT('Origin',(-1.9,-3.,6.9));
#8979=CARTESIAN_POINT('',(-2.175,-0.0249999999999999,6.9));
#8980=CARTESIAN_POINT('',(-2.175,-3.1,6.9));
#8981=CARTESIAN_POINT('Origin',(-1.9,-0.0249999999999999,6.9));
#8982=CARTESIAN_POINT('Origin',(-1.9,-3.1,3.1));
#8983=CARTESIAN_POINT('',(-2.175,-3.,3.1));
#8984=CARTESIAN_POINT('Origin',(-1.9,-3.,3.1));
#8985=CARTESIAN_POINT('',(-2.175,-0.0249999999999999,3.1));
#8986=CARTESIAN_POINT('',(-2.175,-3.1,3.1));
#8987=CARTESIAN_POINT('Origin',(-1.9,-0.0249999999999999,3.1));
#8988=CARTESIAN_POINT('Origin',(1.9,-3.1,6.9));
#8989=CARTESIAN_POINT('',(1.625,-3.,6.9));
#8990=CARTESIAN_POINT('Origin',(1.9,-3.,6.9));
#8991=CARTESIAN_POINT('',(1.625,-0.0249999999999999,6.9));
#8992=CARTESIAN_POINT('',(1.625,-3.1,6.9));
#8993=CARTESIAN_POINT('Origin',(1.9,-0.0249999999999999,6.9));
#8994=CARTESIAN_POINT('Origin',(0.,0.,6.5));
#8995=CARTESIAN_POINT('',(0.699553428981661,-0.025,6.5));
#8996=CARTESIAN_POINT('',(0.699553428981661,-0.025,7.5));
#8997=CARTESIAN_POINT('',(0.699553428981661,-0.025,6.5));
#8998=CARTESIAN_POINT('',(-0.699553428981661,-0.025,6.5));
#8999=CARTESIAN_POINT('Origin',(0.,0.,6.5));
#9000=CARTESIAN_POINT('',(-0.699553428981661,-0.025,7.5));
#9001=CARTESIAN_POINT('',(-0.699553428981661,-0.025,6.5));
#9002=CARTESIAN_POINT('Origin',(0.,0.,7.5));
#9003=CARTESIAN_POINT('Origin',(0.,0.,6.5));
#9004=CARTESIAN_POINT('',(0.556214886532175,-0.025,6.5));
#9005=CARTESIAN_POINT('',(1.25,-0.025,6.5));
#9006=CARTESIAN_POINT('',(-0.556214886532175,-0.025,6.5));
#9007=CARTESIAN_POINT('Origin',(0.,0.,6.5));
#9008=CARTESIAN_POINT('',(1.25,-0.025,6.5));
#9009=CARTESIAN_POINT('Origin',(0.,-1.5125,7.5));
#9010=CARTESIAN_POINT('',(-2.5,-0.025,7.5));
#9011=CARTESIAN_POINT('',(2.5,-0.025,7.5));
#9012=CARTESIAN_POINT('',(-2.5,-3.,7.5));
#9013=CARTESIAN_POINT('',(-2.5,-0.025,7.5));
#9014=CARTESIAN_POINT('',(2.5,-3.,7.5));
#9015=CARTESIAN_POINT('',(-2.5,-3.,7.5));
#9016=CARTESIAN_POINT('',(2.5,-0.025,7.5));
#9017=CARTESIAN_POINT('',(2.5,-3.,7.5));
#9018=CARTESIAN_POINT('',(2.5,-0.025,7.5));
#9019=CARTESIAN_POINT('Origin',(0.,-3.1,5.));
#9020=CARTESIAN_POINT('',(-0.93,-3.,5.));
#9021=CARTESIAN_POINT('Origin',(0.,-3.,5.));
#9022=CARTESIAN_POINT('',(-0.93,-1.8,5.));
#9023=CARTESIAN_POINT('',(-0.93,-3.1,5.));
#9024=CARTESIAN_POINT('Origin',(0.,-1.8,5.));
#9025=CARTESIAN_POINT('Origin',(0.,-1.8,5.));
#9026=CARTESIAN_POINT('',(-1.3,-1.8,5.));
#9027=CARTESIAN_POINT('Origin',(0.,-1.8,5.));
#9028=CARTESIAN_POINT('',(-1.3,-1.,5.));
#9029=CARTESIAN_POINT('',(-1.3,-1.8,5.));
#9030=CARTESIAN_POINT('Origin',(0.,-1.,5.));
#9031=CARTESIAN_POINT('Origin',(0.,-1.,5.));
#9032=CARTESIAN_POINT('',(-1.52958336188405E-16,-1.,6.24899959967968));
#9033=CARTESIAN_POINT('Origin',(0.,-1.,5.));
#9034=CARTESIAN_POINT('Origin',(0.,-1.8,5.));
#9035=CARTESIAN_POINT('Origin',(0.,0.,5.));
#9036=CARTESIAN_POINT('Origin',(0.,-0.025,5.));
#9037=CARTESIAN_POINT('Origin',(2.5,-0.025,2.5));
#9038=CARTESIAN_POINT('',(2.5,-0.025,2.5));
#9039=CARTESIAN_POINT('',(2.5,-0.025,2.5));
#9040=CARTESIAN_POINT('',(-2.5,-0.025,2.5));
#9041=CARTESIAN_POINT('',(2.5,-0.025,2.5));
#9042=CARTESIAN_POINT('',(-2.5,-0.025,2.5));
#9043=CARTESIAN_POINT('Origin',(2.5,-3.,2.5));
#9044=CARTESIAN_POINT('',(2.5,-3.,2.5));
#9045=CARTESIAN_POINT('',(2.5,-3.,2.5));
#9046=CARTESIAN_POINT('',(2.5,-3.,2.5));
#9047=CARTESIAN_POINT('Origin',(-2.5,-3.,2.5));
#9048=CARTESIAN_POINT('',(-2.5,-3.,2.5));
#9049=CARTESIAN_POINT('',(-2.5,-3.,2.5));
#9050=CARTESIAN_POINT('',(-2.5,-3.,2.5));
#9051=CARTESIAN_POINT('Origin',(-2.5,-0.025,2.5));
#9052=CARTESIAN_POINT('',(-2.5,-0.025,2.5));
#9053=CARTESIAN_POINT('Origin',(0.,-1.5125,2.5));
#9054=CARTESIAN_POINT('',(0.,0.,0.));
#9055=CARTESIAN_POINT('Origin',(-1.3,1.,6.8));
#9056=CARTESIAN_POINT('',(-1.465,1.,6.8));
#9057=CARTESIAN_POINT('Origin',(-1.3,1.,6.8));
#9058=CARTESIAN_POINT('',(-1.465,1.,7.5));
#9059=CARTESIAN_POINT('',(-1.465,1.,6.8));
#9060=CARTESIAN_POINT('Origin',(-1.3,1.,7.5));
#9061=CARTESIAN_POINT('Origin',(-1.3,1.,6.8));
#9062=CARTESIAN_POINT('Origin',(1.3,1.,6.8));
#9063=CARTESIAN_POINT('',(1.135,1.,6.8));
#9064=CARTESIAN_POINT('Origin',(1.3,1.,6.8));
#9065=CARTESIAN_POINT('',(1.135,1.,7.5));
#9066=CARTESIAN_POINT('',(1.135,1.,6.8));
#9067=CARTESIAN_POINT('Origin',(1.3,1.,7.5));
#9068=CARTESIAN_POINT('Origin',(1.3,1.,6.8));
#9069=CARTESIAN_POINT('Origin',(1.9,-3.1,3.1));
#9070=CARTESIAN_POINT('',(1.625,0.0249999999999999,3.1));
#9071=CARTESIAN_POINT('Origin',(1.9,0.0249999999999999,3.1));
#9072=CARTESIAN_POINT('',(1.625,3.,3.1));
#9073=CARTESIAN_POINT('',(1.625,-3.1,3.1));
#9074=CARTESIAN_POINT('Origin',(1.9,3.,3.1));
#9075=CARTESIAN_POINT('Origin',(-1.9,-3.1,6.9));
#9076=CARTESIAN_POINT('',(-2.175,0.0249999999999999,6.9));
#9077=CARTESIAN_POINT('Origin',(-1.9,0.0249999999999999,6.9));
#9078=CARTESIAN_POINT('',(-2.175,3.,6.9));
#9079=CARTESIAN_POINT('',(-2.175,-3.1,6.9));
#9080=CARTESIAN_POINT('Origin',(-1.9,3.,6.9));
#9081=CARTESIAN_POINT('Origin',(-1.9,-3.1,3.1));
#9082=CARTESIAN_POINT('',(-2.175,0.0249999999999999,3.1));
#9083=CARTESIAN_POINT('Origin',(-1.9,0.0249999999999999,3.1));
#9084=CARTESIAN_POINT('',(-2.175,3.,3.1));
#9085=CARTESIAN_POINT('',(-2.175,-3.1,3.1));
#9086=CARTESIAN_POINT('Origin',(-1.9,3.,3.1));
#9087=CARTESIAN_POINT('Origin',(1.9,-3.1,6.9));
#9088=CARTESIAN_POINT('',(1.625,0.0249999999999999,6.9));
#9089=CARTESIAN_POINT('Origin',(1.9,0.0249999999999999,6.9));
#9090=CARTESIAN_POINT('',(1.625,3.,6.9));
#9091=CARTESIAN_POINT('',(1.625,-3.1,6.9));
#9092=CARTESIAN_POINT('Origin',(1.9,3.,6.9));
#9093=CARTESIAN_POINT('Origin',(0.,0.,6.5));
#9094=CARTESIAN_POINT('',(-0.699553428981661,0.025,6.5));
#9095=CARTESIAN_POINT('',(-0.699553428981661,0.025,7.5));
#9096=CARTESIAN_POINT('',(-0.699553428981661,0.025,6.5));
#9097=CARTESIAN_POINT('',(0.699553428981661,0.025,6.5));
#9098=CARTESIAN_POINT('Origin',(0.,0.,6.5));
#9099=CARTESIAN_POINT('',(0.699553428981661,0.025,7.5));
#9100=CARTESIAN_POINT('',(0.699553428981661,0.025,6.5));
#9101=CARTESIAN_POINT('Origin',(0.,0.,7.5));
#9102=CARTESIAN_POINT('Origin',(0.,0.,6.5));
#9103=CARTESIAN_POINT('',(-0.556214886532175,0.025,6.5));
#9104=CARTESIAN_POINT('',(-1.25,0.025,6.5));
#9105=CARTESIAN_POINT('',(0.556214886532175,0.025,6.5));
#9106=CARTESIAN_POINT('Origin',(0.,0.,6.5));
#9107=CARTESIAN_POINT('',(-1.25,0.025,6.5));
#9108=CARTESIAN_POINT('Origin',(0.,1.5125,7.5));
#9109=CARTESIAN_POINT('',(2.5,0.0249999999999999,7.5));
#9110=CARTESIAN_POINT('',(-2.5,0.025,7.5));
#9111=CARTESIAN_POINT('',(2.5,3.,7.5));
#9112=CARTESIAN_POINT('',(2.5,0.025,7.5));
#9113=CARTESIAN_POINT('',(-2.5,3.,7.5));
#9114=CARTESIAN_POINT('',(2.5,3.,7.5));
#9115=CARTESIAN_POINT('',(-2.5,0.0249999999999999,7.5));
#9116=CARTESIAN_POINT('',(-2.5,3.,7.5));
#9117=CARTESIAN_POINT('',(-2.5,0.025,7.5));
#9118=CARTESIAN_POINT('Origin',(0.,1.8,5.));
#9119=CARTESIAN_POINT('',(-0.93,1.8,5.));
#9120=CARTESIAN_POINT('Origin',(0.,1.8,5.));
#9121=CARTESIAN_POINT('',(-0.93,3.,5.));
#9122=CARTESIAN_POINT('',(-0.93,1.8,5.));
#9123=CARTESIAN_POINT('Origin',(0.,3.,5.));
#9124=CARTESIAN_POINT('Origin',(0.,1.,5.));
#9125=CARTESIAN_POINT('',(-1.3,1.,5.));
#9126=CARTESIAN_POINT('Origin',(0.,1.,5.));
#9127=CARTESIAN_POINT('',(-1.3,1.8,5.));
#9128=CARTESIAN_POINT('',(-1.3,1.,5.));
#9129=CARTESIAN_POINT('Origin',(0.,1.8,5.));
#9130=CARTESIAN_POINT('Origin',(0.,1.8,5.));
#9131=CARTESIAN_POINT('Origin',(0.,1.,5.));
#9132=CARTESIAN_POINT('',(-1.52958336188405E-16,1.,3.75100040032032));
#9133=CARTESIAN_POINT('Origin',(0.,1.,5.));
#9134=CARTESIAN_POINT('Origin',(0.,0.,5.));
#9135=CARTESIAN_POINT('Origin',(0.,0.025,5.));
#9136=CARTESIAN_POINT('Origin',(2.5,3.,2.5));
#9137=CARTESIAN_POINT('',(2.5,3.,2.5));
#9138=CARTESIAN_POINT('',(-2.5,3.,2.5));
#9139=CARTESIAN_POINT('',(2.5,3.,2.5));
#9140=CARTESIAN_POINT('',(-2.5,3.,2.5));
#9141=CARTESIAN_POINT('',(2.5,3.,2.5));
#9142=CARTESIAN_POINT('Origin',(2.5,0.025,2.5));
#9143=CARTESIAN_POINT('',(2.5,0.025,2.5));
#9144=CARTESIAN_POINT('',(2.5,0.025,2.5));
#9145=CARTESIAN_POINT('',(2.5,0.025,2.5));
#9146=CARTESIAN_POINT('Origin',(-2.5,0.025,2.5));
#9147=CARTESIAN_POINT('',(-2.5,0.0249999999999999,2.5));
#9148=CARTESIAN_POINT('',(-2.5,0.0249999999999999,2.5));
#9149=CARTESIAN_POINT('',(-2.5,0.025,2.5));
#9150=CARTESIAN_POINT('Origin',(-2.5,3.,2.5));
#9151=CARTESIAN_POINT('',(-2.5,3.,2.5));
#9152=CARTESIAN_POINT('Origin',(0.,1.5125,2.5));
#9153=CARTESIAN_POINT('',(0.,0.,0.));
#9154=CARTESIAN_POINT('Origin',(1.9,-0.1,3.1));
#9155=CARTESIAN_POINT('',(1.625,-0.025,3.1));
#9156=CARTESIAN_POINT('Origin',(1.9,-0.025,3.1));
#9157=CARTESIAN_POINT('',(1.625,0.025,3.1));
#9158=CARTESIAN_POINT('',(1.625,-0.1,3.1));
#9159=CARTESIAN_POINT('Origin',(1.9,0.025,3.1));
#9160=CARTESIAN_POINT('Origin',(-1.9,-0.1,6.9));
#9161=CARTESIAN_POINT('',(-2.175,-0.025,6.9));
#9162=CARTESIAN_POINT('Origin',(-1.9,-0.025,6.9));
#9163=CARTESIAN_POINT('',(-2.175,0.025,6.9));
#9164=CARTESIAN_POINT('',(-2.175,-0.1,6.9));
#9165=CARTESIAN_POINT('Origin',(-1.9,0.025,6.9));
#9166=CARTESIAN_POINT('Origin',(-1.9,-0.1,3.1));
#9167=CARTESIAN_POINT('',(-2.175,-0.025,3.1));
#9168=CARTESIAN_POINT('Origin',(-1.9,-0.025,3.1));
#9169=CARTESIAN_POINT('',(-2.175,0.025,3.1));
#9170=CARTESIAN_POINT('',(-2.175,-0.1,3.1));
#9171=CARTESIAN_POINT('Origin',(-1.9,0.025,3.1));
#9172=CARTESIAN_POINT('Origin',(1.9,-0.1,6.9));
#9173=CARTESIAN_POINT('',(1.625,-0.025,6.9));
#9174=CARTESIAN_POINT('Origin',(1.9,-0.025,6.9));
#9175=CARTESIAN_POINT('',(1.625,0.025,6.9));
#9176=CARTESIAN_POINT('',(1.625,-0.1,6.9));
#9177=CARTESIAN_POINT('Origin',(1.9,0.025,6.9));
#9178=CARTESIAN_POINT('Origin',(-0.7,-0.1,6.5));
#9179=CARTESIAN_POINT('',(-0.7,-0.025,6.5));
#9180=CARTESIAN_POINT('',(-0.7,-0.025,7.5));
#9181=CARTESIAN_POINT('',(-0.7,-0.025,5.75));
#9182=CARTESIAN_POINT('',(-0.7,0.025,6.5));
#9183=CARTESIAN_POINT('',(-0.7,-0.1,6.5));
#9184=CARTESIAN_POINT('',(-0.7,0.025,7.5));
#9185=CARTESIAN_POINT('',(-0.7,0.025,5.75));
#9186=CARTESIAN_POINT('',(-0.7,-0.0625,7.5));
#9187=CARTESIAN_POINT('Origin',(0.7,-0.1,6.5));
#9188=CARTESIAN_POINT('',(0.7,-0.025,6.5));
#9189=CARTESIAN_POINT('',(0.556776436283003,-0.025,6.5));
#9190=CARTESIAN_POINT('',(0.35,-0.025,6.5));
#9191=CARTESIAN_POINT('',(0.7,0.025,6.5));
#9192=CARTESIAN_POINT('',(0.7,-0.1,6.5));
#9193=CARTESIAN_POINT('',(0.556776436283003,0.025,6.5));
#9194=CARTESIAN_POINT('',(0.35,0.025,6.5));
#9195=CARTESIAN_POINT('',(0.556776436283003,-0.1,6.5));
#9196=CARTESIAN_POINT('Origin',(0.7,-0.1,6.5));
#9197=CARTESIAN_POINT('',(-0.556776436283003,-0.025,6.5));
#9198=CARTESIAN_POINT('',(0.35,-0.025,6.5));
#9199=CARTESIAN_POINT('',(-0.556776436283003,0.025,6.5));
#9200=CARTESIAN_POINT('',(-0.556776436283003,-0.1,6.5));
#9201=CARTESIAN_POINT('',(0.35,0.025,6.5));
#9202=CARTESIAN_POINT('Origin',(0.7,-0.1,7.6));
#9203=CARTESIAN_POINT('',(0.7,-0.025,7.5));
#9204=CARTESIAN_POINT('',(0.7,-0.025,6.3));
#9205=CARTESIAN_POINT('',(0.7,0.025,7.5));
#9206=CARTESIAN_POINT('',(0.7,-0.0625,7.5));
#9207=CARTESIAN_POINT('',(0.7,0.025,6.3));
#9208=CARTESIAN_POINT('Origin',(0.,0.025,5.));
#9209=CARTESIAN_POINT('Origin',(0.,0.025,5.));
#9210=CARTESIAN_POINT('',(2.5,0.025,7.5));
#9211=CARTESIAN_POINT('',(2.5,0.025,7.5));
#9212=CARTESIAN_POINT('',(2.5,0.025,2.5));
#9213=CARTESIAN_POINT('',(2.5,0.025,2.5));
#9214=CARTESIAN_POINT('',(-2.5,0.025,2.5));
#9215=CARTESIAN_POINT('',(-2.5,0.025,2.5));
#9216=CARTESIAN_POINT('',(-2.5,0.025,7.5));
#9217=CARTESIAN_POINT('',(-2.5,0.025,7.5));
#9218=CARTESIAN_POINT('',(2.5,0.025,7.5));
#9219=CARTESIAN_POINT('Origin',(-2.5,-0.025,7.5));
#9220=CARTESIAN_POINT('',(2.5,-0.025,7.5));
#9221=CARTESIAN_POINT('',(2.5,-0.025,7.5));
#9222=CARTESIAN_POINT('',(2.5,-0.025,7.5));
#9223=CARTESIAN_POINT('Origin',(-2.5,-0.025,7.5));
#9224=CARTESIAN_POINT('',(-2.5,-0.025,7.5));
#9225=CARTESIAN_POINT('',(-2.5,-0.025,7.5));
#9226=CARTESIAN_POINT('',(2.5,-0.025,7.5));
#9227=CARTESIAN_POINT('Origin',(0.,-0.1,5.));
#9228=CARTESIAN_POINT('Origin',(0.,-0.025,5.));
#9229=CARTESIAN_POINT('Origin',(-2.5,-0.025,2.5));
#9230=CARTESIAN_POINT('',(-2.5,-0.025,2.5));
#9231=CARTESIAN_POINT('',(-2.5,-0.025,7.5));
#9232=CARTESIAN_POINT('',(-2.5,-0.025,2.5));
#9233=CARTESIAN_POINT('Origin',(2.5,-0.025,2.5));
#9234=CARTESIAN_POINT('',(2.5,-0.025,2.5));
#9235=CARTESIAN_POINT('',(-2.5,-0.025,2.5));
#9236=CARTESIAN_POINT('',(2.5,-0.025,2.5));
#9237=CARTESIAN_POINT('Origin',(2.5,-0.025,7.5));
#9238=CARTESIAN_POINT('',(2.5,-0.025,2.5));
#9239=CARTESIAN_POINT('Origin',(0.,-0.025,5.));
#9240=CARTESIAN_POINT('',(0.,0.,0.));
#9241=CARTESIAN_POINT('Origin',(0.,0.,7.5));
#9242=CARTESIAN_POINT('',(-1.2,-1.46957615897682E-16,7.5));
#9243=CARTESIAN_POINT('Origin',(0.,0.,7.5));
#9244=CARTESIAN_POINT('',(-0.7,-8.57252759403147E-17,7.5));
#9245=CARTESIAN_POINT('Origin',(0.,0.,7.5));
#9246=CARTESIAN_POINT('Origin',(0.,0.,7.5));
#9247=CARTESIAN_POINT('',(-1.2,-1.46957615897682E-16,8.));
#9248=CARTESIAN_POINT('Origin',(0.,0.,8.));
#9249=CARTESIAN_POINT('',(-1.2,-1.46957615897682E-16,7.5));
#9250=CARTESIAN_POINT('Origin',(0.,0.,8.));
#9251=CARTESIAN_POINT('',(-0.405,-4.95981953654678E-17,8.));
#9252=CARTESIAN_POINT('Origin',(0.,0.,8.));
#9253=CARTESIAN_POINT('Origin',(0.,0.,6.6));
#9254=CARTESIAN_POINT('',(-0.405,-4.95981953654678E-17,6.6));
#9255=CARTESIAN_POINT('',(-0.405,-4.95981953654678E-17,6.6));
#9256=CARTESIAN_POINT('Origin',(0.,0.,6.6));
#9257=CARTESIAN_POINT('Origin',(0.,0.,6.6));
#9258=CARTESIAN_POINT('',(-0.7,-8.57252759403147E-17,6.6));
#9259=CARTESIAN_POINT('',(-0.7,-8.57252759403147E-17,6.6));
#9260=CARTESIAN_POINT('Origin',(0.,0.,6.6));
#9261=CARTESIAN_POINT('Origin',(0.,0.,6.6));
#9262=CARTESIAN_POINT('',(0.,0.,0.));
#9263=CARTESIAN_POINT('Origin',(0.,0.,8.1));
#9264=CARTESIAN_POINT('',(-0.4,-4.89858719658941E-17,8.1));
#9265=CARTESIAN_POINT('Origin',(-0.5,-6.12323399573677E-17,8.1));
#9266=CARTESIAN_POINT('Origin',(0.,0.,8.1));
#9267=CARTESIAN_POINT('',(0.,0.,0.));
#9268=CARTESIAN_POINT('Origin',(0.,0.,7.9));
#9269=CARTESIAN_POINT('',(-0.61,-7.47034547479885E-17,8.));
#9270=CARTESIAN_POINT('Origin',(0.,0.,8.));
#9271=CARTESIAN_POINT('',(-0.61,-7.47034547479885E-17,8.3));
#9272=CARTESIAN_POINT('',(-0.61,-7.47034547479885E-17,7.9));
#9273=CARTESIAN_POINT('Origin',(0.,0.,8.3));
#9274=CARTESIAN_POINT('Origin',(0.,0.,8.3));
#9275=CARTESIAN_POINT('',(-0.405,4.95981953654678E-17,8.3));
#9276=CARTESIAN_POINT('Origin',(0.,0.,8.3));
#9277=CARTESIAN_POINT('Origin',(0.,0.,8.));
#9278=CARTESIAN_POINT('',(-0.405,-4.95981953654678E-17,8.7));
#9279=CARTESIAN_POINT('Origin',(0.,0.,8.7));
#9280=CARTESIAN_POINT('',(-0.405,-4.95981953654678E-17,8.));
#9281=CARTESIAN_POINT('Origin',(0.,0.,8.));
#9282=CARTESIAN_POINT('',(-1.,-1.22464679914735E-16,8.7));
#9283=CARTESIAN_POINT('Origin',(0.,0.,8.7));
#9284=CARTESIAN_POINT('',(-1.,-1.22464679914735E-16,8.));
#9285=CARTESIAN_POINT('',(-1.,-1.22464679914735E-16,8.));
#9286=CARTESIAN_POINT('Origin',(0.,0.,8.));
#9287=CARTESIAN_POINT('Origin',(0.,0.,8.7));
#9288=CARTESIAN_POINT('Origin',(0.,0.,8.));
#9289=CARTESIAN_POINT('',(0.,0.,0.));
#9290=CARTESIAN_POINT('Origin',(-1.1,-3.,8.1));
#9291=CARTESIAN_POINT('',(-1.4,-3.,8.1));
#9292=CARTESIAN_POINT('Origin',(-1.1,-3.,8.1));
#9293=CARTESIAN_POINT('',(-1.4,-3.,8.5));
#9294=CARTESIAN_POINT('',(-1.4,-3.,8.1));
#9295=CARTESIAN_POINT('Origin',(-1.1,-3.,8.5));
#9296=CARTESIAN_POINT('Origin',(-1.1,-3.,8.1));
#9297=CARTESIAN_POINT('Origin',(3.,1.1,8.1));
#9298=CARTESIAN_POINT('',(2.7,1.1,8.1));
#9299=CARTESIAN_POINT('Origin',(3.,1.1,8.1));
#9300=CARTESIAN_POINT('',(2.7,1.1,8.5));
#9301=CARTESIAN_POINT('',(2.7,1.1,8.1));
#9302=CARTESIAN_POINT('Origin',(3.,1.1,8.5));
#9303=CARTESIAN_POINT('Origin',(3.,1.1,8.1));
#9304=CARTESIAN_POINT('Origin',(1.3,-1.,7.9));
#9305=CARTESIAN_POINT('',(1.075,-1.,8.));
#9306=CARTESIAN_POINT('Origin',(1.3,-1.,8.));
#9307=CARTESIAN_POINT('',(1.075,-1.,8.5));
#9308=CARTESIAN_POINT('',(1.075,-1.,7.9));
#9309=CARTESIAN_POINT('Origin',(1.3,-1.,8.5));
#9310=CARTESIAN_POINT('Origin',(-1.3,1.,7.9));
#9311=CARTESIAN_POINT('',(-1.525,1.,8.));
#9312=CARTESIAN_POINT('Origin',(-1.3,1.,8.));
#9313=CARTESIAN_POINT('',(-1.525,1.,8.5));
#9314=CARTESIAN_POINT('',(-1.525,1.,7.9));
#9315=CARTESIAN_POINT('Origin',(-1.3,1.,8.5));
#9316=CARTESIAN_POINT('Origin',(-1.3,-1.,7.9));
#9317=CARTESIAN_POINT('',(-1.525,-1.,8.));
#9318=CARTESIAN_POINT('Origin',(-1.3,-1.,8.));
#9319=CARTESIAN_POINT('',(-1.525,-1.,8.5));
#9320=CARTESIAN_POINT('',(-1.525,-1.,7.9));
#9321=CARTESIAN_POINT('Origin',(-1.3,-1.,8.5));
#9322=CARTESIAN_POINT('Origin',(1.3,1.,7.9));
#9323=CARTESIAN_POINT('',(1.075,1.,8.));
#9324=CARTESIAN_POINT('Origin',(1.3,1.,8.));
#9325=CARTESIAN_POINT('',(1.075,1.,8.5));
#9326=CARTESIAN_POINT('',(1.075,1.,7.9));
#9327=CARTESIAN_POINT('Origin',(1.3,1.,8.5));
#9328=CARTESIAN_POINT('Origin',(0.,0.,7.9));
#9329=CARTESIAN_POINT('',(-1.01,-1.23689326713883E-16,8.));
#9330=CARTESIAN_POINT('Origin',(0.,0.,8.));
#9331=CARTESIAN_POINT('',(-1.01,1.23689326713883E-16,8.5));
#9332=CARTESIAN_POINT('',(-1.01,-1.23689326713883E-16,7.9));
#9333=CARTESIAN_POINT('Origin',(0.,0.,8.5));
#9334=CARTESIAN_POINT('Origin',(4.,1.5,8.));
#9335=CARTESIAN_POINT('',(4.,1.5,8.));
#9336=CARTESIAN_POINT('',(-2.5,1.5,8.));
#9337=CARTESIAN_POINT('',(4.,1.5,8.));
#9338=CARTESIAN_POINT('',(-2.5,1.5,8.5));
#9339=CARTESIAN_POINT('',(-2.5,1.5,8.));
#9340=CARTESIAN_POINT('',(4.,1.5,8.5));
#9341=CARTESIAN_POINT('',(4.,1.5,8.5));
#9342=CARTESIAN_POINT('',(4.,1.5,8.));
#9343=CARTESIAN_POINT('Origin',(4.,-4.,8.));
#9344=CARTESIAN_POINT('',(4.,-4.,8.));
#9345=CARTESIAN_POINT('',(4.,-4.,8.));
#9346=CARTESIAN_POINT('',(4.,-4.,8.5));
#9347=CARTESIAN_POINT('',(4.,-4.,8.5));
#9348=CARTESIAN_POINT('',(4.,-4.,8.));
#9349=CARTESIAN_POINT('Origin',(-2.5,-4.,8.));
#9350=CARTESIAN_POINT('',(-2.5,-4.,8.));
#9351=CARTESIAN_POINT('',(-2.5,-4.,8.));
#9352=CARTESIAN_POINT('',(-2.5,-4.,8.5));
#9353=CARTESIAN_POINT('',(-2.5,-4.,8.5));
#9354=CARTESIAN_POINT('',(-2.5,-4.,8.));
#9355=CARTESIAN_POINT('Origin',(-2.5,1.5,8.));
#9356=CARTESIAN_POINT('',(-2.5,1.5,8.));
#9357=CARTESIAN_POINT('',(-2.5,1.5,8.5));
#9358=CARTESIAN_POINT('Origin',(0.75,-1.25,8.5));
#9359=CARTESIAN_POINT('Origin',(0.75,-1.25,8.));
#9360=CARTESIAN_POINT('',(0.,0.,0.));
#9361=CARTESIAN_POINT('Origin',(0.,0.,5.));
#9362=CARTESIAN_POINT('',(-1.36919674566051E-16,-1.,6.11803398874989));
#9363=CARTESIAN_POINT('Origin',(0.,-1.,5.));
#9364=CARTESIAN_POINT('',(-0.75,-1.29903810567666,5.));
#9365=CARTESIAN_POINT('Origin',(0.,-1.29903810567666,5.));
#9366=CARTESIAN_POINT('Origin',(0.,-1.8,5.));
#9367=CARTESIAN_POINT('',(-0.75,-1.8,5.));
#9368=CARTESIAN_POINT('',(-0.75,-1.8,5.));
#9369=CARTESIAN_POINT('Origin',(0.,-1.8,5.));
#9370=CARTESIAN_POINT('Origin',(0.,-1.8,5.));
#9371=CARTESIAN_POINT('',(-1.3,-1.,5.));
#9372=CARTESIAN_POINT('Origin',(0.,-1.,5.));
#9373=CARTESIAN_POINT('',(-1.3,-1.8,5.));
#9374=CARTESIAN_POINT('',(-1.3,-1.8,5.));
#9375=CARTESIAN_POINT('Origin',(0.,-1.8,5.));
#9376=CARTESIAN_POINT('Origin',(0.,-1.,5.));
#9377=CARTESIAN_POINT('Origin',(0.,-1.8,5.));
#9378=CARTESIAN_POINT('',(0.,0.,0.));
#9379=CARTESIAN_POINT('Origin',(0.115470053837925,-0.5,-0.2));
#9380=CARTESIAN_POINT('',(0.23094010767585,-0.5,0.));
#9381=CARTESIAN_POINT('',(0.115470053837925,-0.5,-0.2));
#9382=CARTESIAN_POINT('',(0.23094010767585,-0.5,0.));
#9383=CARTESIAN_POINT('',(0.115470053837925,-0.8,-0.2));
#9384=CARTESIAN_POINT('',(0.115470053837925,-0.5,-0.2));
#9385=CARTESIAN_POINT('',(0.23094010767585,-0.8,0.));
#9386=CARTESIAN_POINT('',(0.23094010767585,-0.8,0.));
#9387=CARTESIAN_POINT('',(0.23094010767585,-0.5,0.));
#9388=CARTESIAN_POINT('Origin',(-0.115470053837925,-0.5,-0.2));
#9389=CARTESIAN_POINT('',(-0.115470053837925,-0.5,-0.2));
#9390=CARTESIAN_POINT('',(0.115470053837925,-0.5,-0.2));
#9391=CARTESIAN_POINT('',(-0.115470053837925,-0.8,-0.2));
#9392=CARTESIAN_POINT('',(-0.115470053837925,-0.5,-0.2));
#9393=CARTESIAN_POINT('',(0.115470053837925,-0.8,-0.2));
#9394=CARTESIAN_POINT('Origin',(-0.23094010767585,-0.5,-2.77555756156289E-17));
#9395=CARTESIAN_POINT('',(-0.23094010767585,-0.5,-2.82820063659975E-17));
#9396=CARTESIAN_POINT('',(-0.115470053837925,-0.5,-0.2));
#9397=CARTESIAN_POINT('',(-0.23094010767585,-0.8,-2.77555756156289E-17));
#9398=CARTESIAN_POINT('',(-0.23094010767585,-0.5,-2.82820063659975E-17));
#9399=CARTESIAN_POINT('',(-0.115470053837925,-0.8,-0.2));
#9400=CARTESIAN_POINT('Origin',(-0.115470053837925,-0.5,0.2));
#9401=CARTESIAN_POINT('',(-0.115470053837925,-0.5,0.2));
#9402=CARTESIAN_POINT('',(-0.23094010767585,-0.5,-2.82820063659975E-17));
#9403=CARTESIAN_POINT('',(-0.115470053837925,-0.8,0.2));
#9404=CARTESIAN_POINT('',(-0.115470053837925,-0.5,0.2));
#9405=CARTESIAN_POINT('',(-0.23094010767585,-0.8,-2.82820063659975E-17));
#9406=CARTESIAN_POINT('Origin',(0.115470053837925,-0.5,0.2));
#9407=CARTESIAN_POINT('',(0.115470053837925,-0.5,0.2));
#9408=CARTESIAN_POINT('',(-0.115470053837925,-0.5,0.2));
#9409=CARTESIAN_POINT('',(0.115470053837925,-0.8,0.2));
#9410=CARTESIAN_POINT('',(0.115470053837925,-0.5,0.2));
#9411=CARTESIAN_POINT('',(-0.115470053837925,-0.8,0.2));
#9412=CARTESIAN_POINT('Origin',(0.23094010767585,-0.5,0.));
#9413=CARTESIAN_POINT('',(0.115470053837925,-0.5,0.2));
#9414=CARTESIAN_POINT('',(0.115470053837925,-0.8,0.2));
#9415=CARTESIAN_POINT('Origin',(0.,-0.5,0.));
#9416=CARTESIAN_POINT('Origin',(0.,-0.8,0.));
#9417=CARTESIAN_POINT('Origin',(0.,-1.9,0.));
#9418=CARTESIAN_POINT('',(-0.25,-1.9,3.06161699786838E-17));
#9419=CARTESIAN_POINT('Origin',(0.,-1.9,0.));
#9420=CARTESIAN_POINT('',(-0.24505,-1.9,3.00099698131059E-17));
#9421=CARTESIAN_POINT('Origin',(0.,-1.9,0.));
#9422=CARTESIAN_POINT('Origin',(0.,-7.,0.));
#9423=CARTESIAN_POINT('',(-0.25,-7.,3.06161699786838E-17));
#9424=CARTESIAN_POINT('',(-0.25,-7.,3.06161699786838E-17));
#9425=CARTESIAN_POINT('Origin',(0.,-7.,0.));
#9426=CARTESIAN_POINT('Origin',(0.,-7.,0.));
#9427=CARTESIAN_POINT('Origin',(0.375,0.5,0.));
#9428=CARTESIAN_POINT('',(-0.375,0.5,-4.59242549680257E-17));
#9429=CARTESIAN_POINT('Origin',(0.,0.5,0.));
#9430=CARTESIAN_POINT('Origin',(0.,0.475,0.));
#9431=CARTESIAN_POINT('',(-0.425,0.45,-5.20474889637625E-17));
#9432=CARTESIAN_POINT('Origin',(0.,0.45,0.));
#9433=CARTESIAN_POINT('',(-0.4,0.475,-4.89858719658941E-17));
#9434=CARTESIAN_POINT('Origin',(0.,0.24,0.));
#9435=CARTESIAN_POINT('',(-0.425,0.0299999999999998,-5.20474889637625E-17));
#9436=CARTESIAN_POINT('Origin',(0.,0.0299999999999998,0.));
#9437=CARTESIAN_POINT('',(-0.425,0.24,-5.20474889637625E-17));
#9438=CARTESIAN_POINT('Origin',(0.,0.0150000000000001,0.));
#9439=CARTESIAN_POINT('',(-0.395,4.85722573273506E-17,-4.83735485663204E-17));
#9440=CARTESIAN_POINT('Origin',(0.,0.,0.));
#9441=CARTESIAN_POINT('',(-0.41,0.0150000000000001,-5.02105187650415E-17));
#9442=CARTESIAN_POINT('Origin',(0.27,0.,0.));
#9443=CARTESIAN_POINT('',(-0.27,0.,-3.30654635769785E-17));
#9444=CARTESIAN_POINT('Origin',(0.,0.,0.));
#9445=CARTESIAN_POINT('Origin',(0.,-0.02,0.));
#9446=CARTESIAN_POINT('',(-0.24505,-0.0498999999999999,3.00099698131059E-17));
#9447=CARTESIAN_POINT('Origin',(0.,-0.0498999999999999,0.));
#9448=CARTESIAN_POINT('',(-0.26,-0.02,-3.18408167778312E-17));
#9449=CARTESIAN_POINT('Origin',(0.,-0.995,0.));
#9450=CARTESIAN_POINT('',(-0.24505,-0.995,-3.00099698131059E-17));
#9451=CARTESIAN_POINT('',(0.,0.,0.));
#9452=CARTESIAN_POINT('Origin',(0.,0.09,0.));
#9453=CARTESIAN_POINT('',(-0.285,0.1,3.49024337756996E-17));
#9454=CARTESIAN_POINT('Origin',(0.,0.1,0.));
#9455=CARTESIAN_POINT('',(-0.265,0.08,-3.24531401774049E-17));
#9456=CARTESIAN_POINT('',(-0.275,0.09,3.36777869765522E-17));
#9457=CARTESIAN_POINT('Origin',(0.,0.08,0.));
#9458=CARTESIAN_POINT('Origin',(0.,0.,0.));
#9459=CARTESIAN_POINT('',(-0.265,0.,3.24531401774049E-17));
#9460=CARTESIAN_POINT('',(-0.265,0.,3.24531401774049E-17));
#9461=CARTESIAN_POINT('Origin',(0.,0.,0.));
#9462=CARTESIAN_POINT('Origin',(0.,0.1,0.));
#9463=CARTESIAN_POINT('',(-0.5,0.1,6.12323399573677E-17));
#9464=CARTESIAN_POINT('Origin',(0.,0.1,0.));
#9465=CARTESIAN_POINT('Origin',(0.,0.,0.));
#9466=CARTESIAN_POINT('',(-0.5,0.,6.12323399573677E-17));
#9467=CARTESIAN_POINT('',(-0.5,0.,6.12323399573677E-17));
#9468=CARTESIAN_POINT('Origin',(0.,0.,0.));
#9469=CARTESIAN_POINT('Origin',(0.,0.,0.));
#9470=CARTESIAN_POINT('',(0.,0.,0.));
#9471=CARTESIAN_POINT('Origin',(0.,0.0525042956467857,0.));
#9472=CARTESIAN_POINT('',(-0.230940107675851,0.0472735643746089,0.4));
#9473=CARTESIAN_POINT('',(0.23094010767585,0.0472735643746089,0.4));
#9474=CARTESIAN_POINT('Ctrl Pts',(-0.230940107675851,0.0472735643746089,
0.4));
#9475=CARTESIAN_POINT('Ctrl Pts',(1.11022302462516E-16,-0.0193931022920578,
0.4));
#9476=CARTESIAN_POINT('Ctrl Pts',(0.23094010767585,0.0472735643746089,0.4));
#9477=CARTESIAN_POINT('',(-0.461880215351701,0.0472735643746089,-5.6564012731995E-17));
#9478=CARTESIAN_POINT('Ctrl Pts',(-0.461880215351701,0.0472735643746089,
-5.6564012731995E-17));
#9479=CARTESIAN_POINT('Ctrl Pts',(-0.346410161513776,-0.0193931022920579,
0.2));
#9480=CARTESIAN_POINT('Ctrl Pts',(-0.230940107675851,0.0472735643746089,
0.4));
#9481=CARTESIAN_POINT('',(-0.38,-2.08166817117217E-17,-4.65365783675994E-17));
#9482=CARTESIAN_POINT('',(-0.47094010767585,0.0525042956467857,-5.7673529545534E-17));
#9483=CARTESIAN_POINT('Origin',(0.,0.,0.));
#9484=CARTESIAN_POINT('',(-0.23094010767585,0.0472735643746089,-0.4));
#9485=CARTESIAN_POINT('Ctrl Pts',(-0.23094010767585,0.0472735643746089,
-0.4));
#9486=CARTESIAN_POINT('Ctrl Pts',(-0.346410161513775,-0.0193931022920578,
-0.2));
#9487=CARTESIAN_POINT('Ctrl Pts',(-0.461880215351701,0.0472735643746089,
-5.6564012731995E-17));
#9488=CARTESIAN_POINT('',(0.23094010767585,0.0472735643746089,-0.4));
#9489=CARTESIAN_POINT('Ctrl Pts',(0.23094010767585,0.0472735643746089,-0.4));
#9490=CARTESIAN_POINT('Ctrl Pts',(0.,-0.0193931022920578,-0.4));
#9491=CARTESIAN_POINT('Ctrl Pts',(-0.23094010767585,0.0472735643746089,
-0.4));
#9492=CARTESIAN_POINT('',(0.461880215351701,0.0472735643746089,0.));
#9493=CARTESIAN_POINT('Ctrl Pts',(0.461880215351701,0.0472735643746089,
0.));
#9494=CARTESIAN_POINT('Ctrl Pts',(0.346410161513776,-0.019393102292058,
-0.2));
#9495=CARTESIAN_POINT('Ctrl Pts',(0.23094010767585,0.0472735643746089,-0.4));
#9496=CARTESIAN_POINT('Ctrl Pts',(0.23094010767585,0.0472735643746089,0.4));
#9497=CARTESIAN_POINT('Ctrl Pts',(0.346410161513776,-0.0193931022920577,
0.2));
#9498=CARTESIAN_POINT('Ctrl Pts',(0.461880215351701,0.0472735643746089,
0.));
#9499=CARTESIAN_POINT('Origin',(0.,0.417495704353214,0.));
#9500=CARTESIAN_POINT('',(-0.38,0.47,-4.65365783675994E-17));
#9501=CARTESIAN_POINT('Origin',(0.,0.47,0.));
#9502=CARTESIAN_POINT('',(-0.461880215351701,0.422726435625391,-5.6564012731995E-17));
#9503=CARTESIAN_POINT('',(-0.47094010767585,0.417495704353214,-5.7673529545534E-17));
#9504=CARTESIAN_POINT('',(-0.230940107675851,0.422726435625391,0.4));
#9505=CARTESIAN_POINT('Ctrl Pts',(-0.230940107675851,0.422726435625391,
0.4));
#9506=CARTESIAN_POINT('Ctrl Pts',(-0.346410161513776,0.489393102292058,
0.2));
#9507=CARTESIAN_POINT('Ctrl Pts',(-0.461880215351701,0.422726435625391,
-5.6564012731995E-17));
#9508=CARTESIAN_POINT('',(0.23094010767585,0.422726435625391,0.4));
#9509=CARTESIAN_POINT('Ctrl Pts',(0.23094010767585,0.422726435625391,0.4));
#9510=CARTESIAN_POINT('Ctrl Pts',(8.32667268468867E-17,0.489393102292058,
0.4));
#9511=CARTESIAN_POINT('Ctrl Pts',(-0.230940107675851,0.422726435625391,
0.4));
#9512=CARTESIAN_POINT('',(0.461880215351701,0.422726435625391,0.));
#9513=CARTESIAN_POINT('Ctrl Pts',(0.461880215351701,0.422726435625391,0.));
#9514=CARTESIAN_POINT('Ctrl Pts',(0.346410161513776,0.489393102292058,0.2));
#9515=CARTESIAN_POINT('Ctrl Pts',(0.23094010767585,0.422726435625391,0.4));
#9516=CARTESIAN_POINT('',(0.23094010767585,0.422726435625391,-0.4));
#9517=CARTESIAN_POINT('Ctrl Pts',(0.23094010767585,0.422726435625391,-0.4));
#9518=CARTESIAN_POINT('Ctrl Pts',(0.346410161513775,0.489393102292058,-0.2));
#9519=CARTESIAN_POINT('Ctrl Pts',(0.461880215351701,0.422726435625391,0.));
#9520=CARTESIAN_POINT('',(-0.23094010767585,0.422726435625391,-0.4));
#9521=CARTESIAN_POINT('Ctrl Pts',(-0.23094010767585,0.422726435625391,-0.4));
#9522=CARTESIAN_POINT('Ctrl Pts',(-5.55111512312578E-17,0.489393102292058,
-0.4));
#9523=CARTESIAN_POINT('Ctrl Pts',(0.23094010767585,0.422726435625391,-0.4));
#9524=CARTESIAN_POINT('Ctrl Pts',(-0.461880215351701,0.422726435625391,
-5.6564012731995E-17));
#9525=CARTESIAN_POINT('Ctrl Pts',(-0.346410161513776,0.489393102292058,
-0.2));
#9526=CARTESIAN_POINT('Ctrl Pts',(-0.23094010767585,0.422726435625391,-0.4));
#9527=CARTESIAN_POINT('Origin',(0.23094010767585,0.,-0.4));
#9528=CARTESIAN_POINT('',(-0.23094010767585,0.,-0.4));
#9529=CARTESIAN_POINT('',(0.23094010767585,0.,-0.4));
#9530=CARTESIAN_POINT('Origin',(-0.23094010767585,0.,-0.4));
#9531=CARTESIAN_POINT('',(-0.461880215351701,0.,-5.6564012731995E-17));
#9532=CARTESIAN_POINT('Origin',(-0.461880215351701,0.,-5.6564012731995E-17));
#9533=CARTESIAN_POINT('',(-0.230940107675851,0.,0.4));
#9534=CARTESIAN_POINT('Origin',(0.,0.,0.));
#9535=CARTESIAN_POINT('',(-0.2117,0.47,2.59257727379495E-17));
#9536=CARTESIAN_POINT('Origin',(0.,0.47,0.));
#9537=CARTESIAN_POINT('',(-0.2117,0.,2.59257727379495E-17));
#9538=CARTESIAN_POINT('',(-0.2117,0.,2.59257727379495E-17));
#9539=CARTESIAN_POINT('Origin',(0.,0.,0.));
#9540=CARTESIAN_POINT('Origin',(-0.230940107675851,0.,0.4));
#9541=CARTESIAN_POINT('',(0.23094010767585,0.,0.4));
#9542=CARTESIAN_POINT('Origin',(0.461880215351701,0.,0.));
#9543=CARTESIAN_POINT('',(0.461880215351701,0.,0.));
#9544=CARTESIAN_POINT('Origin',(0.23094010767585,0.,0.4));
#9545=CARTESIAN_POINT('Origin',(0.,0.47,0.));
#9546=CARTESIAN_POINT('Origin',(0.,0.,0.));
#9547=CARTESIAN_POINT('',(0.,0.,0.));
#9548=CARTESIAN_POINT('Origin',(0.,-0.6,0.));
#9549=CARTESIAN_POINT('',(1.55884572681199,-0.6,0.));
#9550=CARTESIAN_POINT('',(0.779422863405995,-0.6,1.35));
#9551=CARTESIAN_POINT('',(0.779422863405995,-0.6,1.35));
#9552=CARTESIAN_POINT('',(-0.779422863405996,-0.6,1.35));
#9553=CARTESIAN_POINT('',(-0.779422863405996,-0.6,1.35));
#9554=CARTESIAN_POINT('',(-1.55884572681199,-0.6,-1.90903542970483E-16));
#9555=CARTESIAN_POINT('',(-1.55884572681199,-0.6,-1.90903542970483E-16));
#9556=CARTESIAN_POINT('',(-0.779422863405995,-0.6,-1.35));
#9557=CARTESIAN_POINT('',(-0.779422863405995,-0.6,-1.35));
#9558=CARTESIAN_POINT('',(0.779422863405995,-0.6,-1.35));
#9559=CARTESIAN_POINT('',(0.779422863405995,-0.6,-1.35));
#9560=CARTESIAN_POINT('',(1.55884572681199,-0.6,0.));
#9561=CARTESIAN_POINT('',(-1.065,-0.6,-1.30424884109193E-16));
#9562=CARTESIAN_POINT('Origin',(0.,-0.6,0.));
#9563=CARTESIAN_POINT('Origin',(0.,0.6,0.));
#9564=CARTESIAN_POINT('',(0.779422863405995,0.6,1.35));
#9565=CARTESIAN_POINT('',(1.55884572681199,0.6,0.));
#9566=CARTESIAN_POINT('',(0.779422863405995,0.6,1.35));
#9567=CARTESIAN_POINT('',(0.779422863405995,0.6,-1.35));
#9568=CARTESIAN_POINT('',(1.55884572681199,0.6,0.));
#9569=CARTESIAN_POINT('',(-0.779422863405995,0.6,-1.35));
#9570=CARTESIAN_POINT('',(0.779422863405995,0.6,-1.35));
#9571=CARTESIAN_POINT('',(-1.55884572681199,0.6,-1.90903542970483E-16));
#9572=CARTESIAN_POINT('',(-0.779422863405995,0.6,-1.35));
#9573=CARTESIAN_POINT('',(-0.779422863405996,0.6,1.35));
#9574=CARTESIAN_POINT('',(-1.55884572681199,0.6,-1.90903542970483E-16));
#9575=CARTESIAN_POINT('',(-0.779422863405996,0.6,1.35));
#9576=CARTESIAN_POINT('',(-1.065,0.6,1.30424884109193E-16));
#9577=CARTESIAN_POINT('Origin',(0.,0.6,0.));
#9578=CARTESIAN_POINT('Origin',(-0.779422863405996,0.,1.35));
#9579=CARTESIAN_POINT('',(0.779422863405995,0.,1.35));
#9580=CARTESIAN_POINT('',(-0.779422863405996,0.,1.35));
#9581=CARTESIAN_POINT('Origin',(-1.55884572681199,0.,-1.90903542970483E-16));
#9582=CARTESIAN_POINT('',(-1.55884572681199,0.,-1.90903542970483E-16));
#9583=CARTESIAN_POINT('Origin',(-0.779422863405995,0.,-1.35));
#9584=CARTESIAN_POINT('',(-0.779422863405995,0.,-1.35));
#9585=CARTESIAN_POINT('Origin',(0.779422863405995,0.,-1.35));
#9586=CARTESIAN_POINT('',(0.779422863405995,0.,-1.35));
#9587=CARTESIAN_POINT('Origin',(1.55884572681199,0.,0.));
#9588=CARTESIAN_POINT('',(1.55884572681199,0.,0.));
#9589=CARTESIAN_POINT('Origin',(0.779422863405995,0.,1.35));
#9590=CARTESIAN_POINT('Origin',(0.,0.,0.));
#9591=CARTESIAN_POINT('',(-1.065,2.47,-1.30424884109193E-16));
#9592=CARTESIAN_POINT('',(-1.065,0.,-1.30424884109193E-16));
#9593=CARTESIAN_POINT('Origin',(0.,2.47,0.));
#9594=CARTESIAN_POINT('Origin',(0.985,2.55,0.));
#9595=CARTESIAN_POINT('',(-0.985,2.55,-1.20627709716014E-16));
#9596=CARTESIAN_POINT('Origin',(0.,2.55,0.));
#9597=CARTESIAN_POINT('',(-0.79,2.55,-9.67470971326409E-17));
#9598=CARTESIAN_POINT('Origin',(0.,2.55,0.));
#9599=CARTESIAN_POINT('Origin',(0.,2.51,0.));
#9600=CARTESIAN_POINT('',(-1.025,2.51,-1.25526296912604E-16));
#9601=CARTESIAN_POINT('Origin',(0.,0.,0.));
#9602=CARTESIAN_POINT('',(-1.065,-2.47,-1.30424884109193E-16));
#9603=CARTESIAN_POINT('Origin',(0.,-2.47,0.));
#9604=CARTESIAN_POINT('',(-1.065,0.,-1.30424884109193E-16));
#9605=CARTESIAN_POINT('Origin',(0.,-2.51,0.));
#9606=CARTESIAN_POINT('',(-0.985,-2.55,-1.20627709716014E-16));
#9607=CARTESIAN_POINT('Origin',(0.,-2.55,0.));
#9608=CARTESIAN_POINT('',(-1.025,-2.51,-1.25526296912604E-16));
#9609=CARTESIAN_POINT('Origin',(0.79,-2.55,0.));
#9610=CARTESIAN_POINT('',(-0.79,-2.55,-9.67470971326409E-17));
#9611=CARTESIAN_POINT('Origin',(0.,-2.55,0.));
#9612=CARTESIAN_POINT('Origin',(0.,0.,0.));
#9613=CARTESIAN_POINT('',(-0.79,0.,-9.67470971326409E-17));
#9614=CARTESIAN_POINT('',(0.,0.,0.));
#9615=CARTESIAN_POINT('Origin',(-1.3,-1.,7.5));
#9616=CARTESIAN_POINT('',(-1.525,-1.,8.));
#9617=CARTESIAN_POINT('Origin',(-1.3,-1.,8.));
#9618=CARTESIAN_POINT('',(-1.525,-1.,7.5));
#9619=CARTESIAN_POINT('',(-1.525,-1.,7.5));
#9620=CARTESIAN_POINT('Origin',(-1.3,-1.,7.5));
#9621=CARTESIAN_POINT('Origin',(-1.3,-1.,7.5));
#9622=CARTESIAN_POINT('',(-1.7,-1.,8.));
#9623=CARTESIAN_POINT('Origin',(-1.3,-1.,8.));
#9624=CARTESIAN_POINT('',(-1.7,-1.,7.5));
#9625=CARTESIAN_POINT('',(-1.7,-1.,7.5));
#9626=CARTESIAN_POINT('Origin',(-1.3,-1.,7.5));
#9627=CARTESIAN_POINT('Origin',(-1.3,-1.,8.));
#9628=CARTESIAN_POINT('Origin',(-1.3,-1.,7.5));
#9629=CARTESIAN_POINT('',(0.,0.,0.));
#9630=CARTESIAN_POINT('Origin',(0.3,0.4,0.));
#9631=CARTESIAN_POINT('',(-0.3,0.4,-3.67394039744206E-17));
#9632=CARTESIAN_POINT('Origin',(0.,0.4,0.));
#9633=CARTESIAN_POINT('Origin',(0.,0.375,0.));
#9634=CARTESIAN_POINT('',(-0.35,0.35,-4.28626379701573E-17));
#9635=CARTESIAN_POINT('Origin',(0.,0.35,0.));
#9636=CARTESIAN_POINT('',(-0.325,0.375,-3.9801020972289E-17));
#9637=CARTESIAN_POINT('Origin',(0.,0.19,0.));
#9638=CARTESIAN_POINT('',(-0.35,0.03,-4.28626379701574E-17));
#9639=CARTESIAN_POINT('Origin',(0.,0.03,0.));
#9640=CARTESIAN_POINT('',(-0.35,0.19,-4.28626379701574E-17));
#9641=CARTESIAN_POINT('Origin',(0.,0.0149999999999999,0.));
#9642=CARTESIAN_POINT('',(-0.32,-3.29597460435593E-17,-3.91886975727153E-17));
#9643=CARTESIAN_POINT('Origin',(0.,0.,0.));
#9644=CARTESIAN_POINT('',(-0.335,0.0149999999999999,-4.10256677714363E-17));
#9645=CARTESIAN_POINT('Origin',(0.22,0.,0.));
#9646=CARTESIAN_POINT('',(-0.22,-6.93889390390723E-18,-2.69422295812418E-17));
#9647=CARTESIAN_POINT('Origin',(0.,0.,0.));
#9648=CARTESIAN_POINT('Origin',(0.,-0.02,0.));
#9649=CARTESIAN_POINT('',(-0.1954,-0.0492,2.39295984553393E-17));
#9650=CARTESIAN_POINT('Origin',(0.,-0.0492,0.));
#9651=CARTESIAN_POINT('',(-0.21,-0.02,-2.57175827820944E-17));
#9652=CARTESIAN_POINT('Origin',(0.,-0.8,0.));
#9653=CARTESIAN_POINT('',(-0.1954,-1.5646,2.39295984553393E-17));
#9654=CARTESIAN_POINT('Origin',(0.,-1.5646,0.));
#9655=CARTESIAN_POINT('',(-0.1954,-0.8,-2.39295984553393E-17));
#9656=CARTESIAN_POINT('Origin',(0.,-1.58,0.));
#9657=CARTESIAN_POINT('',(-0.16,-1.6,-1.95943487863577E-17));
#9658=CARTESIAN_POINT('Origin',(0.,-1.6,0.));
#9659=CARTESIAN_POINT('',(-0.18,-1.58,-2.20436423846524E-17));
#9660=CARTESIAN_POINT('Origin',(0.,-1.6,0.));
#9661=CARTESIAN_POINT('Origin',(0.0866025403784439,-0.4,-0.15));
#9662=CARTESIAN_POINT('',(0.173205080756888,-0.4,0.));
#9663=CARTESIAN_POINT('',(0.0866025403784439,-0.4,-0.15));
#9664=CARTESIAN_POINT('',(0.173205080756888,-0.4,0.));
#9665=CARTESIAN_POINT('',(0.0866025403784439,-0.64,-0.15));
#9666=CARTESIAN_POINT('',(0.0866025403784439,-0.4,-0.15));
#9667=CARTESIAN_POINT('',(0.173205080756888,-0.64,0.));
#9668=CARTESIAN_POINT('',(0.173205080756888,-0.64,0.));
#9669=CARTESIAN_POINT('',(0.173205080756888,-0.4,0.));
#9670=CARTESIAN_POINT('Origin',(-0.0866025403784438,-0.4,-0.15));
#9671=CARTESIAN_POINT('',(-0.0866025403784438,-0.4,-0.15));
#9672=CARTESIAN_POINT('',(0.0866025403784439,-0.4,-0.15));
#9673=CARTESIAN_POINT('',(-0.0866025403784438,-0.64,-0.15));
#9674=CARTESIAN_POINT('',(-0.0866025403784438,-0.4,-0.15));
#9675=CARTESIAN_POINT('',(0.0866025403784439,-0.64,-0.15));
#9676=CARTESIAN_POINT('Origin',(-0.173205080756888,-0.4,-2.77555756156289E-17));
#9677=CARTESIAN_POINT('',(-0.173205080756888,-0.4,-2.12115047744981E-17));
#9678=CARTESIAN_POINT('',(-0.0866025403784438,-0.4,-0.15));
#9679=CARTESIAN_POINT('',(-0.173205080756888,-0.64,-2.77555756156289E-17));
#9680=CARTESIAN_POINT('',(-0.173205080756888,-0.4,-2.12115047744981E-17));
#9681=CARTESIAN_POINT('',(-0.0866025403784438,-0.64,-0.15));
#9682=CARTESIAN_POINT('Origin',(-0.0866025403784439,-0.4,0.15));
#9683=CARTESIAN_POINT('',(-0.0866025403784439,-0.4,0.15));
#9684=CARTESIAN_POINT('',(-0.173205080756888,-0.4,-2.12115047744981E-17));
#9685=CARTESIAN_POINT('',(-0.0866025403784439,-0.64,0.15));
#9686=CARTESIAN_POINT('',(-0.0866025403784439,-0.4,0.15));
#9687=CARTESIAN_POINT('',(-0.173205080756888,-0.64,-2.12115047744981E-17));
#9688=CARTESIAN_POINT('Origin',(0.0866025403784439,-0.4,0.15));
#9689=CARTESIAN_POINT('',(0.0866025403784439,-0.4,0.15));
#9690=CARTESIAN_POINT('',(-0.0866025403784439,-0.4,0.15));
#9691=CARTESIAN_POINT('',(0.0866025403784439,-0.64,0.15));
#9692=CARTESIAN_POINT('',(0.0866025403784439,-0.4,0.15));
#9693=CARTESIAN_POINT('',(-0.0866025403784439,-0.64,0.15));
#9694=CARTESIAN_POINT('Origin',(0.173205080756888,-0.4,0.));
#9695=CARTESIAN_POINT('',(0.0866025403784439,-0.4,0.15));
#9696=CARTESIAN_POINT('',(0.0866025403784439,-0.64,0.15));
#9697=CARTESIAN_POINT('Origin',(0.,-0.4,-2.77555756156289E-17));
#9698=CARTESIAN_POINT('Origin',(0.,-0.64,-2.77555756156289E-17));
#9699=CARTESIAN_POINT('',(0.,0.,0.));
#9700=CARTESIAN_POINT('Origin',(3.,1.1,8.2));
#9701=CARTESIAN_POINT('',(2.7,1.1,9.4));
#9702=CARTESIAN_POINT('Origin',(3.,1.1,9.4));
#9703=CARTESIAN_POINT('',(2.7,1.1,8.2));
#9704=CARTESIAN_POINT('',(2.7,1.1,8.2));
#9705=CARTESIAN_POINT('Origin',(3.,1.1,8.2));
#9706=CARTESIAN_POINT('Origin',(3.,1.1,9.4));
#9707=CARTESIAN_POINT('Origin',(3.,1.1,8.2));
#9708=CARTESIAN_POINT('',(0.,0.,0.));
#9709=CARTESIAN_POINT('',(0.,0.,0.));
#9710=CARTESIAN_POINT('Origin',(-0.205,-0.205,6.));
#9711=CARTESIAN_POINT('',(0.205,-0.205,6.47171668469172));
#9712=CARTESIAN_POINT('',(-0.205,-0.205,6.47171668469172));
#9713=CARTESIAN_POINT('Origin',(0.,-0.205,5.));
#9714=CARTESIAN_POINT('',(0.205,-0.205,6.));
#9715=CARTESIAN_POINT('',(0.205,-0.205,6.));
#9716=CARTESIAN_POINT('',(-0.205,-0.205,6.));
#9717=CARTESIAN_POINT('',(-0.205,-0.205,6.));
#9718=CARTESIAN_POINT('',(-0.205,-0.205,6.));
#9719=CARTESIAN_POINT('Origin',(-0.205,0.205,6.));
#9720=CARTESIAN_POINT('',(-0.205,-2.51052593825207E-17,6.48592563743951));
#9721=CARTESIAN_POINT('Origin',(-0.205,0.,5.));
#9722=CARTESIAN_POINT('',(-0.205,0.205,6.));
#9723=CARTESIAN_POINT('',(-0.205,0.205,6.));
#9724=CARTESIAN_POINT('',(-0.205,0.205,6.47171668469172));
#9725=CARTESIAN_POINT('',(-0.205,0.205,6.));
#9726=CARTESIAN_POINT('Origin',(-0.205,0.,5.));
#9727=CARTESIAN_POINT('Origin',(0.205,0.205,6.));
#9728=CARTESIAN_POINT('',(0.205,0.205,6.47171668469172));
#9729=CARTESIAN_POINT('Origin',(0.,0.205,5.));
#9730=CARTESIAN_POINT('',(0.205,0.205,6.));
#9731=CARTESIAN_POINT('',(0.205,0.205,6.));
#9732=CARTESIAN_POINT('',(0.205,0.205,6.));
#9733=CARTESIAN_POINT('Origin',(0.205,-0.205,6.));
#9734=CARTESIAN_POINT('Origin',(0.205,0.,5.));
#9735=CARTESIAN_POINT('',(0.205,-0.205,6.));
#9736=CARTESIAN_POINT('Origin',(0.,0.,6.));
#9737=CARTESIAN_POINT('Origin',(0.,-1.6,5.));
#9738=CARTESIAN_POINT('',(-0.75,-1.29903810567666,5.));
#9739=CARTESIAN_POINT('Origin',(0.,-1.29903810567666,5.));
#9740=CARTESIAN_POINT('',(-0.75,1.29903810567666,5.));
#9741=CARTESIAN_POINT('',(-0.75,-1.6,5.));
#9742=CARTESIAN_POINT('Origin',(0.,1.29903810567666,5.));
#9743=CARTESIAN_POINT('Origin',(0.,0.,5.));
#9744=CARTESIAN_POINT('',(-9.18485099360515E-17,-1.12481983699639E-32,3.5));
#9745=CARTESIAN_POINT('Origin',(0.,0.,5.));
#9746=CARTESIAN_POINT('',(0.,0.,0.));
#9747=CARTESIAN_POINT('Origin',(0.,0.,8.5));
#9748=CARTESIAN_POINT('',(-0.165,-2.02066721859313E-17,8.5));
#9749=CARTESIAN_POINT('Origin',(0.,0.,8.5));
#9750=CARTESIAN_POINT('',(-0.165,2.02066721859313E-17,9.4));
#9751=CARTESIAN_POINT('',(-0.165,-2.02066721859313E-17,8.5));
#9752=CARTESIAN_POINT('Origin',(0.,0.,9.4));
#9753=CARTESIAN_POINT('Origin',(0.,0.,8.5));
#9754=CARTESIAN_POINT('Origin',(0.,0.,8.7));
#9755=CARTESIAN_POINT('',(-0.264575131106459,0.3,8.7));
#9756=CARTESIAN_POINT('',(-0.3,0.264575131106459,8.7));
#9757=CARTESIAN_POINT('Origin',(0.,0.,8.7));
#9758=CARTESIAN_POINT('',(-0.3,0.3,8.7));
#9759=CARTESIAN_POINT('',(-0.3,0.3,8.7));
#9760=CARTESIAN_POINT('',(0.3,0.3,8.7));
#9761=CARTESIAN_POINT('Origin',(0.,0.,8.7));
#9762=CARTESIAN_POINT('',(-0.3,-0.264575131106459,8.7));
#9763=CARTESIAN_POINT('',(-0.264575131106459,-0.3,8.7));
#9764=CARTESIAN_POINT('Origin',(0.,0.,8.7));
#9765=CARTESIAN_POINT('',(-0.3,-0.3,8.7));
#9766=CARTESIAN_POINT('',(-0.3,-0.3,8.7));
#9767=CARTESIAN_POINT('',(-0.3,0.3,8.7));
#9768=CARTESIAN_POINT('Origin',(0.,0.,8.7));
#9769=CARTESIAN_POINT('',(0.264575131106459,-0.3,8.7));
#9770=CARTESIAN_POINT('',(0.3,-0.264575131106459,8.7));
#9771=CARTESIAN_POINT('Origin',(0.,0.,8.7));
#9772=CARTESIAN_POINT('',(0.3,-0.3,8.7));
#9773=CARTESIAN_POINT('',(0.3,-0.3,8.7));
#9774=CARTESIAN_POINT('',(-0.3,-0.3,8.7));
#9775=CARTESIAN_POINT('Origin',(0.,0.,8.7));
#9776=CARTESIAN_POINT('',(0.3,0.264575131106459,8.7));
#9777=CARTESIAN_POINT('',(0.264575131106459,0.3,8.7));
#9778=CARTESIAN_POINT('Origin',(0.,0.,8.7));
#9779=CARTESIAN_POINT('',(0.3,0.3,8.7));
#9780=CARTESIAN_POINT('',(0.3,0.3,8.7));
#9781=CARTESIAN_POINT('',(0.3,-0.3,8.7));
#9782=CARTESIAN_POINT('Origin',(0.3,0.3,8.7));
#9783=CARTESIAN_POINT('',(0.15,0.3,8.7));
#9784=CARTESIAN_POINT('',(-0.3,0.3,9.4));
#9785=CARTESIAN_POINT('',(-0.3,0.3,8.7));
#9786=CARTESIAN_POINT('',(0.3,0.3,9.4));
#9787=CARTESIAN_POINT('',(0.3,0.3,9.4));
#9788=CARTESIAN_POINT('',(0.3,0.3,8.7));
#9789=CARTESIAN_POINT('Origin',(0.3,-0.3,8.7));
#9790=CARTESIAN_POINT('',(0.3,-0.15,8.7));
#9791=CARTESIAN_POINT('',(0.3,-0.3,9.4));
#9792=CARTESIAN_POINT('',(0.3,-0.3,9.4));
#9793=CARTESIAN_POINT('',(0.3,-0.3,8.7));
#9794=CARTESIAN_POINT('Origin',(-0.3,-0.3,8.7));
#9795=CARTESIAN_POINT('',(-0.15,-0.3,8.7));
#9796=CARTESIAN_POINT('',(-0.3,-0.3,9.4));
#9797=CARTESIAN_POINT('',(-0.3,-0.3,9.4));
#9798=CARTESIAN_POINT('',(-0.3,-0.3,8.7));
#9799=CARTESIAN_POINT('Origin',(-0.3,0.3,8.7));
#9800=CARTESIAN_POINT('',(-0.3,0.15,8.7));
#9801=CARTESIAN_POINT('',(-0.3,0.3,9.4));
#9802=CARTESIAN_POINT('Origin',(0.,0.,9.4));
#9803=CARTESIAN_POINT('Origin',(0.,0.,8.7));
#9804=CARTESIAN_POINT('Origin',(0.,0.,8.7));
#9805=CARTESIAN_POINT('Origin',(0.,0.,8.7));
#9806=CARTESIAN_POINT('',(-0.4,-4.89858719658941E-17,8.7));
#9807=CARTESIAN_POINT('Origin',(0.,0.,8.7));
#9808=CARTESIAN_POINT('Origin',(0.,0.,8.7));
#9809=CARTESIAN_POINT('Origin',(0.,0.,8.7));
#9810=CARTESIAN_POINT('Origin',(0.,0.,8.7));
#9811=CARTESIAN_POINT('Origin',(0.,0.,8.7));
#9812=CARTESIAN_POINT('Origin',(0.,0.,8.7));
#9813=CARTESIAN_POINT('Origin',(0.2,0.2,6.));
#9814=CARTESIAN_POINT('',(0.2,0.2,6.));
#9815=CARTESIAN_POINT('',(-0.2,0.2,6.));
#9816=CARTESIAN_POINT('',(0.2,0.2,6.));
#9817=CARTESIAN_POINT('',(-0.2,0.2,6.5));
#9818=CARTESIAN_POINT('',(-0.2,0.2,6.));
#9819=CARTESIAN_POINT('',(0.2,0.2,6.5));
#9820=CARTESIAN_POINT('',(0.1,0.2,6.5));
#9821=CARTESIAN_POINT('',(0.2,0.2,6.));
#9822=CARTESIAN_POINT('Origin',(0.2,-0.2,6.));
#9823=CARTESIAN_POINT('',(0.2,-0.2,6.));
#9824=CARTESIAN_POINT('',(0.2,-0.2,6.));
#9825=CARTESIAN_POINT('',(0.2,-0.2,6.5));
#9826=CARTESIAN_POINT('',(0.2,-0.1,6.5));
#9827=CARTESIAN_POINT('',(0.2,-0.2,6.));
#9828=CARTESIAN_POINT('Origin',(-0.2,-0.2,6.));
#9829=CARTESIAN_POINT('',(-0.2,-0.2,6.));
#9830=CARTESIAN_POINT('',(-0.2,-0.2,6.));
#9831=CARTESIAN_POINT('',(-0.2,-0.2,6.5));
#9832=CARTESIAN_POINT('',(-0.1,-0.2,6.5));
#9833=CARTESIAN_POINT('',(-0.2,-0.2,6.));
#9834=CARTESIAN_POINT('Origin',(-0.2,0.2,6.));
#9835=CARTESIAN_POINT('',(-0.2,0.2,6.));
#9836=CARTESIAN_POINT('',(-0.2,0.1,6.5));
#9837=CARTESIAN_POINT('Origin',(0.,0.,6.));
#9838=CARTESIAN_POINT('Origin',(0.,0.,6.5));
#9839=CARTESIAN_POINT('',(-0.4,-4.89858719658941E-17,6.5));
#9840=CARTESIAN_POINT('',(-0.4,-4.89858719658941E-17,6.5));
#9841=CARTESIAN_POINT('Origin',(0.,0.,6.5));
#9842=CARTESIAN_POINT('Origin',(0.,0.,6.5));
#9843=CARTESIAN_POINT('',(0.,0.,0.));
#9844=CARTESIAN_POINT('Origin',(-0.305,-0.305,8.9));
#9845=CARTESIAN_POINT('',(0.305,-0.305,9.4));
#9846=CARTESIAN_POINT('',(-0.305,-0.305,9.4));
#9847=CARTESIAN_POINT('',(1.6475,-0.305,9.4));
#9848=CARTESIAN_POINT('',(0.305,-0.305,9.));
#9849=CARTESIAN_POINT('',(0.305,-0.305,8.9));
#9850=CARTESIAN_POINT('',(-0.305,-0.305,9.));
#9851=CARTESIAN_POINT('',(1.6475,-0.305,9.));
#9852=CARTESIAN_POINT('',(-0.305,-0.305,8.9));
#9853=CARTESIAN_POINT('Origin',(-0.305,0.305,8.9));
#9854=CARTESIAN_POINT('',(-0.305,0.305,9.4));
#9855=CARTESIAN_POINT('',(-0.305,0.1525,9.4));
#9856=CARTESIAN_POINT('',(-0.305,0.305,9.));
#9857=CARTESIAN_POINT('',(-0.305,0.1525,9.));
#9858=CARTESIAN_POINT('',(-0.305,0.305,8.9));
#9859=CARTESIAN_POINT('Origin',(0.305,0.305,8.9));
#9860=CARTESIAN_POINT('',(0.305,0.305,9.4));
#9861=CARTESIAN_POINT('',(1.9525,0.305,9.4));
#9862=CARTESIAN_POINT('',(0.305,0.305,9.));
#9863=CARTESIAN_POINT('',(1.9525,0.305,9.));
#9864=CARTESIAN_POINT('',(0.305,0.305,8.9));
#9865=CARTESIAN_POINT('Origin',(0.305,-0.305,8.9));
#9866=CARTESIAN_POINT('',(0.305,-0.1525,9.4));
#9867=CARTESIAN_POINT('',(0.305,-0.1525,9.));
#9868=CARTESIAN_POINT('Origin',(8.,0.8,9.));
#9869=CARTESIAN_POINT('',(8.,0.8,9.));
#9870=CARTESIAN_POINT('',(-0.8,0.8,9.));
#9871=CARTESIAN_POINT('',(8.,0.8,9.));
#9872=CARTESIAN_POINT('',(-0.8,0.8,9.4));
#9873=CARTESIAN_POINT('',(-0.8,0.8,9.));
#9874=CARTESIAN_POINT('',(8.,0.8,9.4));
#9875=CARTESIAN_POINT('',(8.,0.8,9.4));
#9876=CARTESIAN_POINT('',(8.,0.8,9.));
#9877=CARTESIAN_POINT('Origin',(8.,-0.8,9.));
#9878=CARTESIAN_POINT('',(8.,-0.8,9.));
#9879=CARTESIAN_POINT('',(8.,-0.8,9.));
#9880=CARTESIAN_POINT('',(8.,-0.8,9.4));
#9881=CARTESIAN_POINT('',(8.,-0.8,9.4));
#9882=CARTESIAN_POINT('',(8.,-0.8,9.));
#9883=CARTESIAN_POINT('Origin',(-0.8,-0.8,9.));
#9884=CARTESIAN_POINT('',(-0.8,-0.8,9.));
#9885=CARTESIAN_POINT('',(-0.8,-0.8,9.));
#9886=CARTESIAN_POINT('',(-0.8,-0.8,9.4));
#9887=CARTESIAN_POINT('',(-0.8,-0.8,9.4));
#9888=CARTESIAN_POINT('',(-0.8,-0.8,9.));
#9889=CARTESIAN_POINT('Origin',(-0.8,0.8,9.));
#9890=CARTESIAN_POINT('',(-0.8,0.8,9.));
#9891=CARTESIAN_POINT('',(-0.8,0.8,9.4));
#9892=CARTESIAN_POINT('Origin',(3.6,0.,9.4));
#9893=CARTESIAN_POINT('Origin',(3.6,0.,9.));
#9894=CARTESIAN_POINT('',(0.,0.,0.));
#9895=CARTESIAN_POINT('Origin',(0.,0.,9.4));
#9896=CARTESIAN_POINT('',(-0.225,-2.75545529808154E-17,9.6));
#9897=CARTESIAN_POINT('Origin',(0.,0.,9.6));
#9898=CARTESIAN_POINT('',(-0.225,-2.75545529808154E-17,9.4));
#9899=CARTESIAN_POINT('',(-0.225,-2.75545529808154E-17,9.4));
#9900=CARTESIAN_POINT('Origin',(0.,0.,9.4));
#9901=CARTESIAN_POINT('Origin',(0.,0.,9.4));
#9902=CARTESIAN_POINT('',(-0.6,-7.34788079488412E-17,9.6));
#9903=CARTESIAN_POINT('Origin',(0.,0.,9.6));
#9904=CARTESIAN_POINT('',(-0.6,-7.34788079488412E-17,9.4));
#9905=CARTESIAN_POINT('',(-0.6,-7.34788079488412E-17,9.4));
#9906=CARTESIAN_POINT('Origin',(0.,0.,9.4));
#9907=CARTESIAN_POINT('Origin',(0.,0.,9.6));
#9908=CARTESIAN_POINT('Origin',(0.,0.,9.4));
#9909=CARTESIAN_POINT('',(0.,0.,0.));
#9910=CARTESIAN_POINT('Origin',(8.5,1.,9.4));
#9911=CARTESIAN_POINT('',(8.5,1.,9.4));
#9912=CARTESIAN_POINT('',(6.,1.,9.4));
#9913=CARTESIAN_POINT('',(8.5,1.,9.4));
#9914=CARTESIAN_POINT('',(6.,1.,10.2));
#9915=CARTESIAN_POINT('',(6.,1.,9.4));
#9916=CARTESIAN_POINT('',(8.5,1.,10.2));
#9917=CARTESIAN_POINT('',(8.5,1.,10.2));
#9918=CARTESIAN_POINT('',(8.5,1.,9.4));
#9919=CARTESIAN_POINT('Origin',(8.5,-1.,9.4));
#9920=CARTESIAN_POINT('',(8.5,-1.,9.4));
#9921=CARTESIAN_POINT('',(8.5,-1.,9.4));
#9922=CARTESIAN_POINT('',(8.5,-1.,10.2));
#9923=CARTESIAN_POINT('',(8.5,-1.,10.2));
#9924=CARTESIAN_POINT('',(8.5,-1.,9.4));
#9925=CARTESIAN_POINT('Origin',(6.,-1.,9.4));
#9926=CARTESIAN_POINT('',(6.,-1.,9.4));
#9927=CARTESIAN_POINT('',(6.,-1.,9.4));
#9928=CARTESIAN_POINT('',(6.,-1.,10.2));
#9929=CARTESIAN_POINT('',(6.,-1.,10.2));
#9930=CARTESIAN_POINT('',(6.,-1.,9.4));
#9931=CARTESIAN_POINT('Origin',(6.,1.,9.4));
#9932=CARTESIAN_POINT('',(6.,1.,9.4));
#9933=CARTESIAN_POINT('',(6.,1.,10.2));
#9934=CARTESIAN_POINT('Origin',(7.25,0.,10.2));
#9935=CARTESIAN_POINT('Origin',(7.25,0.,9.4));
#9936=CARTESIAN_POINT('',(0.,0.,0.));
#9937=CARTESIAN_POINT('Origin',(0.0866025403784439,-0.4,-0.15));
#9938=CARTESIAN_POINT('',(0.173205080756888,-0.4,0.));
#9939=CARTESIAN_POINT('',(0.0866025403784439,-0.4,-0.15));
#9940=CARTESIAN_POINT('',(0.173205080756888,-0.4,0.));
#9941=CARTESIAN_POINT('',(0.0866025403784439,-0.64,-0.15));
#9942=CARTESIAN_POINT('',(0.0866025403784439,-0.4,-0.15));
#9943=CARTESIAN_POINT('',(0.173205080756888,-0.64,0.));
#9944=CARTESIAN_POINT('',(0.173205080756888,-0.64,0.));
#9945=CARTESIAN_POINT('',(0.173205080756888,-0.4,0.));
#9946=CARTESIAN_POINT('Origin',(-0.0866025403784438,-0.4,-0.15));
#9947=CARTESIAN_POINT('',(-0.0866025403784438,-0.4,-0.15));
#9948=CARTESIAN_POINT('',(0.0866025403784439,-0.4,-0.15));
#9949=CARTESIAN_POINT('',(-0.0866025403784438,-0.64,-0.15));
#9950=CARTESIAN_POINT('',(-0.0866025403784438,-0.4,-0.15));
#9951=CARTESIAN_POINT('',(0.0866025403784439,-0.64,-0.15));
#9952=CARTESIAN_POINT('Origin',(-0.173205080756888,-0.4,-2.77555756156289E-17));
#9953=CARTESIAN_POINT('',(-0.173205080756888,-0.4,-2.12115047744981E-17));
#9954=CARTESIAN_POINT('',(-0.0866025403784438,-0.4,-0.15));
#9955=CARTESIAN_POINT('',(-0.173205080756888,-0.64,-2.77555756156289E-17));
#9956=CARTESIAN_POINT('',(-0.173205080756888,-0.4,-2.12115047744981E-17));
#9957=CARTESIAN_POINT('',(-0.0866025403784438,-0.64,-0.15));
#9958=CARTESIAN_POINT('Origin',(-0.0866025403784439,-0.4,0.15));
#9959=CARTESIAN_POINT('',(-0.0866025403784439,-0.4,0.15));
#9960=CARTESIAN_POINT('',(-0.173205080756888,-0.4,-2.12115047744981E-17));
#9961=CARTESIAN_POINT('',(-0.0866025403784439,-0.64,0.15));
#9962=CARTESIAN_POINT('',(-0.0866025403784439,-0.4,0.15));
#9963=CARTESIAN_POINT('',(-0.173205080756888,-0.64,-2.12115047744981E-17));
#9964=CARTESIAN_POINT('Origin',(0.0866025403784439,-0.4,0.15));
#9965=CARTESIAN_POINT('',(0.0866025403784439,-0.4,0.15));
#9966=CARTESIAN_POINT('',(-0.0866025403784439,-0.4,0.15));
#9967=CARTESIAN_POINT('',(0.0866025403784439,-0.64,0.15));
#9968=CARTESIAN_POINT('',(0.0866025403784439,-0.4,0.15));
#9969=CARTESIAN_POINT('',(-0.0866025403784439,-0.64,0.15));
#9970=CARTESIAN_POINT('Origin',(0.173205080756888,-0.4,0.));
#9971=CARTESIAN_POINT('',(0.0866025403784439,-0.4,0.15));
#9972=CARTESIAN_POINT('',(0.0866025403784439,-0.64,0.15));
#9973=CARTESIAN_POINT('Origin',(0.,-0.4,-2.77555756156289E-17));
#9974=CARTESIAN_POINT('Origin',(0.,-0.64,-2.77555756156289E-17));
#9975=CARTESIAN_POINT('Origin',(0.,-1.,0.));
#9976=CARTESIAN_POINT('',(-0.1954,-1.,2.39295984553393E-17));
#9977=CARTESIAN_POINT('Origin',(0.,-1.,0.));
#9978=CARTESIAN_POINT('Origin',(0.3,0.4,0.));
#9979=CARTESIAN_POINT('',(-0.3,0.4,-3.67394039744206E-17));
#9980=CARTESIAN_POINT('Origin',(0.,0.4,0.));
#9981=CARTESIAN_POINT('Origin',(0.,0.375,0.));
#9982=CARTESIAN_POINT('',(-0.35,0.35,-4.28626379701573E-17));
#9983=CARTESIAN_POINT('Origin',(0.,0.35,0.));
#9984=CARTESIAN_POINT('',(-0.325,0.375,-3.9801020972289E-17));
#9985=CARTESIAN_POINT('Origin',(0.,0.19,0.));
#9986=CARTESIAN_POINT('',(-0.35,0.03,-4.28626379701574E-17));
#9987=CARTESIAN_POINT('Origin',(0.,0.03,0.));
#9988=CARTESIAN_POINT('',(-0.35,0.19,-4.28626379701574E-17));
#9989=CARTESIAN_POINT('Origin',(0.,0.0149999999999999,0.));
#9990=CARTESIAN_POINT('',(-0.32,-3.29597460435593E-17,-3.91886975727153E-17));
#9991=CARTESIAN_POINT('Origin',(0.,0.,0.));
#9992=CARTESIAN_POINT('',(-0.335,0.0149999999999999,-4.10256677714363E-17));
#9993=CARTESIAN_POINT('Origin',(0.22,0.,0.));
#9994=CARTESIAN_POINT('',(-0.22,-6.93889390390723E-18,-2.69422295812418E-17));
#9995=CARTESIAN_POINT('Origin',(0.,0.,0.));
#9996=CARTESIAN_POINT('Origin',(0.,-0.02,0.));
#9997=CARTESIAN_POINT('',(-0.1954,-0.0492,2.39295984553393E-17));
#9998=CARTESIAN_POINT('Origin',(0.,-0.0492,0.));
#9999=CARTESIAN_POINT('',(-0.21,-0.02,-2.57175827820944E-17));
#10000=CARTESIAN_POINT('Origin',(0.,-0.8,0.));
#10001=CARTESIAN_POINT('',(-0.1954,-0.8,-2.39295984553393E-17));
#10002=CARTESIAN_POINT('',(0.,0.,0.));
#10003=CARTESIAN_POINT('',(0.,0.,0.));
#10004=CARTESIAN_POINT('',(0.,0.,0.));
#10005=CARTESIAN_POINT('',(0.,0.,0.));
#10006=CARTESIAN_POINT('',(0.,0.,0.));
#10007=CARTESIAN_POINT('',(0.,0.,9.6));
#10008=CARTESIAN_POINT('',(0.,0.,0.));
#10009=CARTESIAN_POINT('',(0.,0.,0.));
#10010=CARTESIAN_POINT('',(0.,0.,0.));
#10011=CARTESIAN_POINT('',(0.,0.,0.));
#10012=CARTESIAN_POINT('',(0.,0.,0.));
#10013=CARTESIAN_POINT('',(0.,0.,0.));
#10014=CARTESIAN_POINT('',(0.,0.,0.));
#10015=CARTESIAN_POINT('',(0.,0.,0.));
#10016=CARTESIAN_POINT('',(0.,0.,0.));
#10017=CARTESIAN_POINT('',(-1.9,-3.,3.1));
#10018=CARTESIAN_POINT('',(-1.9,-3.1,3.1));
#10019=CARTESIAN_POINT('',(-1.9,3.,3.1));
#10020=CARTESIAN_POINT('',(-1.9,3.1,3.1));
#10021=CARTESIAN_POINT('',(-1.9,-3.,6.9));
#10022=CARTESIAN_POINT('',(-1.9,-3.1,6.9));
#10023=CARTESIAN_POINT('',(-1.9,3.,6.9));
#10024=CARTESIAN_POINT('',(-1.9,3.1,6.9));
#10025=CARTESIAN_POINT('',(1.9,-3.,3.1));
#10026=CARTESIAN_POINT('',(1.9,-3.1,3.1));
#10027=CARTESIAN_POINT('',(1.9,3.,3.1));
#10028=CARTESIAN_POINT('',(1.9,3.1,3.1));
#10029=CARTESIAN_POINT('',(1.9,-3.,6.9));
#10030=CARTESIAN_POINT('',(1.9,-3.1,6.9));
#10031=CARTESIAN_POINT('',(1.9,3.,6.9));
#10032=CARTESIAN_POINT('',(1.9,3.1,6.9));
#10033=CARTESIAN_POINT('',(0.,-4.35,5.));
#10034=CARTESIAN_POINT('',(0.,4.35,5.));
#10035=CARTESIAN_POINT('',(0.,0.,0.));
#10036=CARTESIAN_POINT('',(-1.3,-1.,8.5));
#10037=CARTESIAN_POINT('',(0.,2.,0.));
#10038=CARTESIAN_POINT('',(-1.3,1.,8.5));
#10039=CARTESIAN_POINT('',(2.6,0.,0.));
#10040=CARTESIAN_POINT('',(1.3,-1.,8.5));
#10041=CARTESIAN_POINT('',(2.6,2.,0.));
#10042=CARTESIAN_POINT('',(1.3,1.,8.5));
#10043=CARTESIAN_POINT('',(0.,0.,0.));
#10044=CARTESIAN_POINT('',(-4.1,-4.1,0.));
#10045=CARTESIAN_POINT('',(0.,0.,0.));
#10046=CARTESIAN_POINT('',(0.,0.,0.));
#10047=CARTESIAN_POINT('',(0.,0.,0.));
#10048=CARTESIAN_POINT('',(0.,0.,0.));
#10049=CARTESIAN_POINT('',(0.,0.,0.));
#10050=CARTESIAN_POINT('',(0.,0.,0.));
#10051=CARTESIAN_POINT('',(41.35,7.75,5.));
#10052=CARTESIAN_POINT('',(-2.5,9.,2.1));
#10053=CARTESIAN_POINT('',(38.5,9.,2.1));
#10054=CARTESIAN_POINT('',(0.,0.,0.));
#10055=CARTESIAN_POINT('',(12.,1.77635683940025E-15,1.77635683940025E-15));
#10056=CARTESIAN_POINT('',(24.,0.,0.));
#10057=CARTESIAN_POINT('',(36.,0.,-1.11022302462516E-16));
#10058=UNCERTAINTY_MEASURE_WITH_UNIT(LENGTH_MEASURE(0.001),#10120,
'DISTANCE_ACCURACY_VALUE',
'Maximum model space distance between geometric entities at asserted c
onnectivities');
#10059=UNCERTAINTY_MEASURE_WITH_UNIT(LENGTH_MEASURE(0.001),#10120,
'DISTANCE_ACCURACY_VALUE',
'Maximum model space distance between geometric entities at asserted c
onnectivities');
#10060=UNCERTAINTY_MEASURE_WITH_UNIT(LENGTH_MEASURE(0.001),#10120,
'DISTANCE_ACCURACY_VALUE',
'Maximum model space distance between geometric entities at asserted c
onnectivities');
#10061=UNCERTAINTY_MEASURE_WITH_UNIT(LENGTH_MEASURE(0.001),#10120,
'DISTANCE_ACCURACY_VALUE',
'Maximum model space distance between geometric entities at asserted c
onnectivities');
#10062=UNCERTAINTY_MEASURE_WITH_UNIT(LENGTH_MEASURE(0.001),#10120,
'DISTANCE_ACCURACY_VALUE',
'Maximum model space distance between geometric entities at asserted c
onnectivities');
#10063=UNCERTAINTY_MEASURE_WITH_UNIT(LENGTH_MEASURE(0.001),#10120,
'DISTANCE_ACCURACY_VALUE',
'Maximum model space distance between geometric entities at asserted c
onnectivities');
#10064=UNCERTAINTY_MEASURE_WITH_UNIT(LENGTH_MEASURE(0.001),#10120,
'DISTANCE_ACCURACY_VALUE',
'Maximum model space distance between geometric entities at asserted c
onnectivities');
#10065=UNCERTAINTY_MEASURE_WITH_UNIT(LENGTH_MEASURE(0.001),#10120,
'DISTANCE_ACCURACY_VALUE',
'Maximum model space distance between geometric entities at asserted c
onnectivities');
#10066=UNCERTAINTY_MEASURE_WITH_UNIT(LENGTH_MEASURE(0.001),#10120,
'DISTANCE_ACCURACY_VALUE',
'Maximum model space distance between geometric entities at asserted c
onnectivities');
#10067=UNCERTAINTY_MEASURE_WITH_UNIT(LENGTH_MEASURE(0.001),#10120,
'DISTANCE_ACCURACY_VALUE',
'Maximum model space distance between geometric entities at asserted c
onnectivities');
#10068=UNCERTAINTY_MEASURE_WITH_UNIT(LENGTH_MEASURE(0.001),#10120,
'DISTANCE_ACCURACY_VALUE',
'Maximum model space distance between geometric entities at asserted c
onnectivities');
#10069=UNCERTAINTY_MEASURE_WITH_UNIT(LENGTH_MEASURE(0.001),#10120,
'DISTANCE_ACCURACY_VALUE',
'Maximum model space distance between geometric entities at asserted c
onnectivities');
#10070=UNCERTAINTY_MEASURE_WITH_UNIT(LENGTH_MEASURE(0.001),#10120,
'DISTANCE_ACCURACY_VALUE',
'Maximum model space distance between geometric entities at asserted c
onnectivities');
#10071=UNCERTAINTY_MEASURE_WITH_UNIT(LENGTH_MEASURE(0.001),#10120,
'DISTANCE_ACCURACY_VALUE',
'Maximum model space distance between geometric entities at asserted c
onnectivities');
#10072=UNCERTAINTY_MEASURE_WITH_UNIT(LENGTH_MEASURE(0.001),#10120,
'DISTANCE_ACCURACY_VALUE',
'Maximum model space distance between geometric entities at asserted c
onnectivities');
#10073=UNCERTAINTY_MEASURE_WITH_UNIT(LENGTH_MEASURE(0.001),#10120,
'DISTANCE_ACCURACY_VALUE',
'Maximum model space distance between geometric entities at asserted c
onnectivities');
#10074=UNCERTAINTY_MEASURE_WITH_UNIT(LENGTH_MEASURE(0.001),#10120,
'DISTANCE_ACCURACY_VALUE',
'Maximum model space distance between geometric entities at asserted c
onnectivities');
#10075=UNCERTAINTY_MEASURE_WITH_UNIT(LENGTH_MEASURE(0.001),#10120,
'DISTANCE_ACCURACY_VALUE',
'Maximum model space distance between geometric entities at asserted c
onnectivities');
#10076=UNCERTAINTY_MEASURE_WITH_UNIT(LENGTH_MEASURE(0.001),#10120,
'DISTANCE_ACCURACY_VALUE',
'Maximum model space distance between geometric entities at asserted c
onnectivities');
#10077=UNCERTAINTY_MEASURE_WITH_UNIT(LENGTH_MEASURE(0.001),#10120,
'DISTANCE_ACCURACY_VALUE',
'Maximum model space distance between geometric entities at asserted c
onnectivities');
#10078=UNCERTAINTY_MEASURE_WITH_UNIT(LENGTH_MEASURE(0.001),#10120,
'DISTANCE_ACCURACY_VALUE',
'Maximum model space distance between geometric entities at asserted c
onnectivities');
#10079=UNCERTAINTY_MEASURE_WITH_UNIT(LENGTH_MEASURE(0.001),#10120,
'DISTANCE_ACCURACY_VALUE',
'Maximum model space distance between geometric entities at asserted c
onnectivities');
#10080=UNCERTAINTY_MEASURE_WITH_UNIT(LENGTH_MEASURE(0.001),#10120,
'DISTANCE_ACCURACY_VALUE',
'Maximum model space distance between geometric entities at asserted c
onnectivities');
#10081=UNCERTAINTY_MEASURE_WITH_UNIT(LENGTH_MEASURE(0.001),#10120,
'DISTANCE_ACCURACY_VALUE',
'Maximum model space distance between geometric entities at asserted c
onnectivities');
#10082=UNCERTAINTY_MEASURE_WITH_UNIT(LENGTH_MEASURE(0.001),#10120,
'DISTANCE_ACCURACY_VALUE',
'Maximum model space distance between geometric entities at asserted c
onnectivities');
#10083=UNCERTAINTY_MEASURE_WITH_UNIT(LENGTH_MEASURE(0.001),#10120,
'DISTANCE_ACCURACY_VALUE',
'Maximum model space distance between geometric entities at asserted c
onnectivities');
#10084=UNCERTAINTY_MEASURE_WITH_UNIT(LENGTH_MEASURE(0.001),#10120,
'DISTANCE_ACCURACY_VALUE',
'Maximum model space distance between geometric entities at asserted c
onnectivities');
#10085=UNCERTAINTY_MEASURE_WITH_UNIT(LENGTH_MEASURE(0.001),#10120,
'DISTANCE_ACCURACY_VALUE',
'Maximum model space distance between geometric entities at asserted c
onnectivities');
#10086=UNCERTAINTY_MEASURE_WITH_UNIT(LENGTH_MEASURE(0.001),#10120,
'DISTANCE_ACCURACY_VALUE',
'Maximum model space distance between geometric entities at asserted c
onnectivities');
#10087=UNCERTAINTY_MEASURE_WITH_UNIT(LENGTH_MEASURE(0.001),#10120,
'DISTANCE_ACCURACY_VALUE',
'Maximum model space distance between geometric entities at asserted c
onnectivities');
#10088=UNCERTAINTY_MEASURE_WITH_UNIT(LENGTH_MEASURE(0.001),#10120,
'DISTANCE_ACCURACY_VALUE',
'Maximum model space distance between geometric entities at asserted c
onnectivities');
#10089=(
GEOMETRIC_REPRESENTATION_CONTEXT(3)
GLOBAL_UNCERTAINTY_ASSIGNED_CONTEXT((#10058))
GLOBAL_UNIT_ASSIGNED_CONTEXT((#10120,#10122,#10123))
REPRESENTATION_CONTEXT('','3D')
);
#10090=(
GEOMETRIC_REPRESENTATION_CONTEXT(3)
GLOBAL_UNCERTAINTY_ASSIGNED_CONTEXT((#10059))
GLOBAL_UNIT_ASSIGNED_CONTEXT((#10120,#10122,#10123))
REPRESENTATION_CONTEXT('','3D')
);
#10091=(
GEOMETRIC_REPRESENTATION_CONTEXT(3)
GLOBAL_UNCERTAINTY_ASSIGNED_CONTEXT((#10060))
GLOBAL_UNIT_ASSIGNED_CONTEXT((#10120,#10122,#10123))
REPRESENTATION_CONTEXT('','3D')
);
#10092=(
GEOMETRIC_REPRESENTATION_CONTEXT(3)
GLOBAL_UNCERTAINTY_ASSIGNED_CONTEXT((#10061))
GLOBAL_UNIT_ASSIGNED_CONTEXT((#10120,#10122,#10123))
REPRESENTATION_CONTEXT('','3D')
);
#10093=(
GEOMETRIC_REPRESENTATION_CONTEXT(3)
GLOBAL_UNCERTAINTY_ASSIGNED_CONTEXT((#10062))
GLOBAL_UNIT_ASSIGNED_CONTEXT((#10120,#10122,#10123))
REPRESENTATION_CONTEXT('','3D')
);
#10094=(
GEOMETRIC_REPRESENTATION_CONTEXT(3)
GLOBAL_UNCERTAINTY_ASSIGNED_CONTEXT((#10063))
GLOBAL_UNIT_ASSIGNED_CONTEXT((#10120,#10122,#10123))
REPRESENTATION_CONTEXT('','3D')
);
#10095=(
GEOMETRIC_REPRESENTATION_CONTEXT(3)
GLOBAL_UNCERTAINTY_ASSIGNED_CONTEXT((#10064))
GLOBAL_UNIT_ASSIGNED_CONTEXT((#10120,#10122,#10123))
REPRESENTATION_CONTEXT('','3D')
);
#10096=(
GEOMETRIC_REPRESENTATION_CONTEXT(3)
GLOBAL_UNCERTAINTY_ASSIGNED_CONTEXT((#10065))
GLOBAL_UNIT_ASSIGNED_CONTEXT((#10120,#10122,#10123))
REPRESENTATION_CONTEXT('','3D')
);
#10097=(
GEOMETRIC_REPRESENTATION_CONTEXT(3)
GLOBAL_UNCERTAINTY_ASSIGNED_CONTEXT((#10066))
GLOBAL_UNIT_ASSIGNED_CONTEXT((#10120,#10122,#10123))
REPRESENTATION_CONTEXT('','3D')
);
#10098=(
GEOMETRIC_REPRESENTATION_CONTEXT(3)
GLOBAL_UNCERTAINTY_ASSIGNED_CONTEXT((#10067))
GLOBAL_UNIT_ASSIGNED_CONTEXT((#10120,#10122,#10123))
REPRESENTATION_CONTEXT('','3D')
);
#10099=(
GEOMETRIC_REPRESENTATION_CONTEXT(3)
GLOBAL_UNCERTAINTY_ASSIGNED_CONTEXT((#10068))
GLOBAL_UNIT_ASSIGNED_CONTEXT((#10120,#10122,#10123))
REPRESENTATION_CONTEXT('','3D')
);
#10100=(
GEOMETRIC_REPRESENTATION_CONTEXT(3)
GLOBAL_UNCERTAINTY_ASSIGNED_CONTEXT((#10069))
GLOBAL_UNIT_ASSIGNED_CONTEXT((#10120,#10122,#10123))
REPRESENTATION_CONTEXT('','3D')
);
#10101=(
GEOMETRIC_REPRESENTATION_CONTEXT(3)
GLOBAL_UNCERTAINTY_ASSIGNED_CONTEXT((#10070))
GLOBAL_UNIT_ASSIGNED_CONTEXT((#10120,#10122,#10123))
REPRESENTATION_CONTEXT('','3D')
);
#10102=(
GEOMETRIC_REPRESENTATION_CONTEXT(3)
GLOBAL_UNCERTAINTY_ASSIGNED_CONTEXT((#10071))
GLOBAL_UNIT_ASSIGNED_CONTEXT((#10120,#10122,#10123))
REPRESENTATION_CONTEXT('','3D')
);
#10103=(
GEOMETRIC_REPRESENTATION_CONTEXT(3)
GLOBAL_UNCERTAINTY_ASSIGNED_CONTEXT((#10072))
GLOBAL_UNIT_ASSIGNED_CONTEXT((#10120,#10122,#10123))
REPRESENTATION_CONTEXT('','3D')
);
#10104=(
GEOMETRIC_REPRESENTATION_CONTEXT(3)
GLOBAL_UNCERTAINTY_ASSIGNED_CONTEXT((#10073))
GLOBAL_UNIT_ASSIGNED_CONTEXT((#10120,#10122,#10123))
REPRESENTATION_CONTEXT('','3D')
);
#10105=(
GEOMETRIC_REPRESENTATION_CONTEXT(3)
GLOBAL_UNCERTAINTY_ASSIGNED_CONTEXT((#10074))
GLOBAL_UNIT_ASSIGNED_CONTEXT((#10120,#10122,#10123))
REPRESENTATION_CONTEXT('','3D')
);
#10106=(
GEOMETRIC_REPRESENTATION_CONTEXT(3)
GLOBAL_UNCERTAINTY_ASSIGNED_CONTEXT((#10075))
GLOBAL_UNIT_ASSIGNED_CONTEXT((#10120,#10122,#10123))
REPRESENTATION_CONTEXT('','3D')
);
#10107=(
GEOMETRIC_REPRESENTATION_CONTEXT(3)
GLOBAL_UNCERTAINTY_ASSIGNED_CONTEXT((#10076))
GLOBAL_UNIT_ASSIGNED_CONTEXT((#10120,#10122,#10123))
REPRESENTATION_CONTEXT('','3D')
);
#10108=(
GEOMETRIC_REPRESENTATION_CONTEXT(3)
GLOBAL_UNCERTAINTY_ASSIGNED_CONTEXT((#10077))
GLOBAL_UNIT_ASSIGNED_CONTEXT((#10120,#10122,#10123))
REPRESENTATION_CONTEXT('','3D')
);
#10109=(
GEOMETRIC_REPRESENTATION_CONTEXT(3)
GLOBAL_UNCERTAINTY_ASSIGNED_CONTEXT((#10078))
GLOBAL_UNIT_ASSIGNED_CONTEXT((#10120,#10122,#10123))
REPRESENTATION_CONTEXT('','3D')
);
#10110=(
GEOMETRIC_REPRESENTATION_CONTEXT(3)
GLOBAL_UNCERTAINTY_ASSIGNED_CONTEXT((#10079))
GLOBAL_UNIT_ASSIGNED_CONTEXT((#10120,#10122,#10123))
REPRESENTATION_CONTEXT('','3D')
);
#10111=(
GEOMETRIC_REPRESENTATION_CONTEXT(3)
GLOBAL_UNCERTAINTY_ASSIGNED_CONTEXT((#10080))
GLOBAL_UNIT_ASSIGNED_CONTEXT((#10120,#10122,#10123))
REPRESENTATION_CONTEXT('','3D')
);
#10112=(
GEOMETRIC_REPRESENTATION_CONTEXT(3)
GLOBAL_UNCERTAINTY_ASSIGNED_CONTEXT((#10081))
GLOBAL_UNIT_ASSIGNED_CONTEXT((#10120,#10122,#10123))
REPRESENTATION_CONTEXT('','3D')
);
#10113=(
GEOMETRIC_REPRESENTATION_CONTEXT(3)
GLOBAL_UNCERTAINTY_ASSIGNED_CONTEXT((#10082))
GLOBAL_UNIT_ASSIGNED_CONTEXT((#10120,#10122,#10123))
REPRESENTATION_CONTEXT('','3D')
);
#10114=(
GEOMETRIC_REPRESENTATION_CONTEXT(3)
GLOBAL_UNCERTAINTY_ASSIGNED_CONTEXT((#10083))
GLOBAL_UNIT_ASSIGNED_CONTEXT((#10120,#10122,#10123))
REPRESENTATION_CONTEXT('','3D')
);
#10115=(
GEOMETRIC_REPRESENTATION_CONTEXT(3)
GLOBAL_UNCERTAINTY_ASSIGNED_CONTEXT((#10084))
GLOBAL_UNIT_ASSIGNED_CONTEXT((#10120,#10122,#10123))
REPRESENTATION_CONTEXT('','3D')
);
#10116=(
GEOMETRIC_REPRESENTATION_CONTEXT(3)
GLOBAL_UNCERTAINTY_ASSIGNED_CONTEXT((#10085))
GLOBAL_UNIT_ASSIGNED_CONTEXT((#10120,#10122,#10123))
REPRESENTATION_CONTEXT('','3D')
);
#10117=(
GEOMETRIC_REPRESENTATION_CONTEXT(3)
GLOBAL_UNCERTAINTY_ASSIGNED_CONTEXT((#10086))
GLOBAL_UNIT_ASSIGNED_CONTEXT((#10120,#10122,#10123))
REPRESENTATION_CONTEXT('','3D')
);
#10118=(
GEOMETRIC_REPRESENTATION_CONTEXT(3)
GLOBAL_UNCERTAINTY_ASSIGNED_CONTEXT((#10087))
GLOBAL_UNIT_ASSIGNED_CONTEXT((#10120,#10122,#10123))
REPRESENTATION_CONTEXT('','3D')
);
#10119=(
GEOMETRIC_REPRESENTATION_CONTEXT(3)
GLOBAL_UNCERTAINTY_ASSIGNED_CONTEXT((#10088))
GLOBAL_UNIT_ASSIGNED_CONTEXT((#10120,#10122,#10123))
REPRESENTATION_CONTEXT('','3D')
);
#10120=(
LENGTH_UNIT()
NAMED_UNIT(*)
SI_UNIT(.CENTI.,.METRE.)
);
#10121=(
LENGTH_UNIT()
NAMED_UNIT(*)
SI_UNIT($,.METRE.)
);
#10122=(
NAMED_UNIT(*)
PLANE_ANGLE_UNIT()
SI_UNIT($,.RADIAN.)
);
#10123=(
NAMED_UNIT(*)
SI_UNIT($,.STERADIAN.)
SOLID_ANGLE_UNIT()
);
#10124=SHAPE_DEFINITION_REPRESENTATION(#10154,#10240);
#10125=SHAPE_DEFINITION_REPRESENTATION(#10155,#10241);
#10126=SHAPE_DEFINITION_REPRESENTATION(#10156,#10242);
#10127=SHAPE_DEFINITION_REPRESENTATION(#10157,#10243);
#10128=SHAPE_DEFINITION_REPRESENTATION(#10158,#10244);
#10129=SHAPE_DEFINITION_REPRESENTATION(#10159,#10245);
#10130=SHAPE_DEFINITION_REPRESENTATION(#10160,#10246);
#10131=SHAPE_DEFINITION_REPRESENTATION(#10161,#10247);
#10132=SHAPE_DEFINITION_REPRESENTATION(#10162,#10248);
#10133=SHAPE_DEFINITION_REPRESENTATION(#10163,#10249);
#10134=SHAPE_DEFINITION_REPRESENTATION(#10164,#10250);
#10135=SHAPE_DEFINITION_REPRESENTATION(#10165,#10251);
#10136=SHAPE_DEFINITION_REPRESENTATION(#10166,#10252);
#10137=SHAPE_DEFINITION_REPRESENTATION(#10167,#10253);
#10138=SHAPE_DEFINITION_REPRESENTATION(#10168,#10254);
#10139=SHAPE_DEFINITION_REPRESENTATION(#10169,#10255);
#10140=SHAPE_DEFINITION_REPRESENTATION(#10170,#10256);
#10141=SHAPE_DEFINITION_REPRESENTATION(#10171,#10257);
#10142=SHAPE_DEFINITION_REPRESENTATION(#10172,#10258);
#10143=SHAPE_DEFINITION_REPRESENTATION(#10173,#10259);
#10144=SHAPE_DEFINITION_REPRESENTATION(#10174,#10260);
#10145=SHAPE_DEFINITION_REPRESENTATION(#10175,#10261);
#10146=SHAPE_DEFINITION_REPRESENTATION(#10176,#10262);
#10147=SHAPE_DEFINITION_REPRESENTATION(#10177,#10263);
#10148=SHAPE_DEFINITION_REPRESENTATION(#10178,#10264);
#10149=SHAPE_DEFINITION_REPRESENTATION(#10179,#10265);
#10150=SHAPE_DEFINITION_REPRESENTATION(#10180,#10266);
#10151=SHAPE_DEFINITION_REPRESENTATION(#10181,#10267);
#10152=SHAPE_DEFINITION_REPRESENTATION(#10182,#10268);
#10153=SHAPE_DEFINITION_REPRESENTATION(#10183,#10269);
#10154=PRODUCT_DEFINITION_SHAPE('',$,#10271);
#10155=PRODUCT_DEFINITION_SHAPE('',$,#10272);
#10156=PRODUCT_DEFINITION_SHAPE('',$,#10273);
#10157=PRODUCT_DEFINITION_SHAPE('',$,#10274);
#10158=PRODUCT_DEFINITION_SHAPE('',$,#10275);
#10159=PRODUCT_DEFINITION_SHAPE('',$,#10276);
#10160=PRODUCT_DEFINITION_SHAPE('',$,#10277);
#10161=PRODUCT_DEFINITION_SHAPE('',$,#10278);
#10162=PRODUCT_DEFINITION_SHAPE('',$,#10279);
#10163=PRODUCT_DEFINITION_SHAPE('',$,#10280);
#10164=PRODUCT_DEFINITION_SHAPE('',$,#10281);
#10165=PRODUCT_DEFINITION_SHAPE('',$,#10282);
#10166=PRODUCT_DEFINITION_SHAPE('',$,#10283);
#10167=PRODUCT_DEFINITION_SHAPE('',$,#10284);
#10168=PRODUCT_DEFINITION_SHAPE('',$,#10285);
#10169=PRODUCT_DEFINITION_SHAPE('',$,#10286);
#10170=PRODUCT_DEFINITION_SHAPE('',$,#10287);
#10171=PRODUCT_DEFINITION_SHAPE('',$,#10288);
#10172=PRODUCT_DEFINITION_SHAPE('',$,#10289);
#10173=PRODUCT_DEFINITION_SHAPE('',$,#10290);
#10174=PRODUCT_DEFINITION_SHAPE('',$,#10291);
#10175=PRODUCT_DEFINITION_SHAPE('',$,#10292);
#10176=PRODUCT_DEFINITION_SHAPE('',$,#10293);
#10177=PRODUCT_DEFINITION_SHAPE('',$,#10294);
#10178=PRODUCT_DEFINITION_SHAPE('',$,#10295);
#10179=PRODUCT_DEFINITION_SHAPE('',$,#10296);
#10180=PRODUCT_DEFINITION_SHAPE('',$,#10297);
#10181=PRODUCT_DEFINITION_SHAPE('',$,#10298);
#10182=PRODUCT_DEFINITION_SHAPE('',$,#10299);
#10183=PRODUCT_DEFINITION_SHAPE('',$,#10300);
#10184=PRODUCT_DEFINITION_SHAPE($,$,#179);
#10185=PRODUCT_DEFINITION_SHAPE($,$,#180);
#10186=PRODUCT_DEFINITION_SHAPE($,$,#181);
#10187=PRODUCT_DEFINITION_SHAPE($,$,#182);
#10188=PRODUCT_DEFINITION_SHAPE($,$,#183);
#10189=PRODUCT_DEFINITION_SHAPE($,$,#184);
#10190=PRODUCT_DEFINITION_SHAPE($,$,#185);
#10191=PRODUCT_DEFINITION_SHAPE($,$,#186);
#10192=PRODUCT_DEFINITION_SHAPE($,$,#187);
#10193=PRODUCT_DEFINITION_SHAPE($,$,#188);
#10194=PRODUCT_DEFINITION_SHAPE($,$,#189);
#10195=PRODUCT_DEFINITION_SHAPE($,$,#190);
#10196=PRODUCT_DEFINITION_SHAPE($,$,#191);
#10197=PRODUCT_DEFINITION_SHAPE($,$,#192);
#10198=PRODUCT_DEFINITION_SHAPE($,$,#193);
#10199=PRODUCT_DEFINITION_SHAPE($,$,#194);
#10200=PRODUCT_DEFINITION_SHAPE($,$,#195);
#10201=PRODUCT_DEFINITION_SHAPE($,$,#196);
#10202=PRODUCT_DEFINITION_SHAPE($,$,#197);
#10203=PRODUCT_DEFINITION_SHAPE($,$,#198);
#10204=PRODUCT_DEFINITION_SHAPE($,$,#199);
#10205=PRODUCT_DEFINITION_SHAPE($,$,#200);
#10206=PRODUCT_DEFINITION_SHAPE($,$,#201);
#10207=PRODUCT_DEFINITION_SHAPE($,$,#202);
#10208=PRODUCT_DEFINITION_SHAPE($,$,#203);
#10209=PRODUCT_DEFINITION_SHAPE($,$,#204);
#10210=PRODUCT_DEFINITION_SHAPE($,$,#205);
#10211=PRODUCT_DEFINITION_SHAPE($,$,#206);
#10212=PRODUCT_DEFINITION_SHAPE($,$,#207);
#10213=PRODUCT_DEFINITION_SHAPE($,$,#208);
#10214=PRODUCT_DEFINITION_SHAPE($,$,#209);
#10215=PRODUCT_DEFINITION_SHAPE($,$,#210);
#10216=PRODUCT_DEFINITION_SHAPE($,$,#211);
#10217=PRODUCT_DEFINITION_SHAPE($,$,#212);
#10218=PRODUCT_DEFINITION_SHAPE($,$,#213);
#10219=PRODUCT_DEFINITION_SHAPE($,$,#214);
#10220=PRODUCT_DEFINITION_SHAPE($,$,#215);
#10221=PRODUCT_DEFINITION_SHAPE($,$,#216);
#10222=PRODUCT_DEFINITION_SHAPE($,$,#217);
#10223=PRODUCT_DEFINITION_SHAPE($,$,#218);
#10224=PRODUCT_DEFINITION_SHAPE($,$,#219);
#10225=PRODUCT_DEFINITION_SHAPE($,$,#220);
#10226=PRODUCT_DEFINITION_SHAPE($,$,#221);
#10227=PRODUCT_DEFINITION_SHAPE($,$,#222);
#10228=PRODUCT_DEFINITION_SHAPE($,$,#223);
#10229=PRODUCT_DEFINITION_SHAPE($,$,#224);
#10230=PRODUCT_DEFINITION_SHAPE($,$,#225);
#10231=PRODUCT_DEFINITION_SHAPE($,$,#226);
#10232=PRODUCT_DEFINITION_SHAPE($,$,#227);
#10233=PRODUCT_DEFINITION_SHAPE($,$,#228);
#10234=PRODUCT_DEFINITION_SHAPE($,$,#229);
#10235=PRODUCT_DEFINITION_SHAPE($,$,#230);
#10236=PRODUCT_DEFINITION_SHAPE($,$,#231);
#10237=PRODUCT_DEFINITION_SHAPE($,$,#232);
#10238=PRODUCT_DEFINITION_SHAPE($,$,#233);
#10239=PRODUCT_DEFINITION_SHAPE($,$,#234);
#10240=SHAPE_REPRESENTATION('',(#5895,#6565,#6566,#6567,#6568),#10089);
#10241=SHAPE_REPRESENTATION('',(#5896,#6557,#6558,#6559,#6560,#6561,#6562,
#6563,#6564),#10090);
#10242=SHAPE_REPRESENTATION('',(#5897),#10091);
#10243=SHAPE_REPRESENTATION('',(#6019),#10092);
#10244=SHAPE_REPRESENTATION('',(#6032),#10093);
#10245=SHAPE_REPRESENTATION('',(#6060),#10094);
#10246=SHAPE_REPRESENTATION('',(#6088),#10095);
#10247=SHAPE_REPRESENTATION('',(#6105,#6519,#6520,#6521,#6522,#6523,#6524,
#6525,#6526,#6527,#6528,#6529,#6530,#6531,#6532,#6533,#6534,#6535,#6536,
#6537,#6538,#6539,#6540,#6541,#6542,#6543,#6544,#6545,#6546,#6547,#6548,
#6549,#6550,#6551,#6552,#6553,#6554,#6555,#6556),#10096);
#10248=SHAPE_REPRESENTATION('',(#6106),#10097);
#10249=SHAPE_REPRESENTATION('',(#6149),#10098);
#10250=SHAPE_REPRESENTATION('',(#6192),#10099);
#10251=SHAPE_REPRESENTATION('',(#6219),#10100);
#10252=SHAPE_REPRESENTATION('',(#6232),#10101);
#10253=SHAPE_REPRESENTATION('',(#6236),#10102);
#10254=SHAPE_REPRESENTATION('',(#6249),#10103);
#10255=SHAPE_REPRESENTATION('',(#6279),#10104);
#10256=SHAPE_REPRESENTATION('',(#6290),#10105);
#10257=SHAPE_REPRESENTATION('',(#6318),#10106);
#10258=SHAPE_REPRESENTATION('',(#6329),#10107);
#10259=SHAPE_REPRESENTATION('',(#6345),#10108);
#10260=SHAPE_REPRESENTATION('',(#6369),#10109);
#10261=SHAPE_REPRESENTATION('',(#6378),#10110);
#10262=SHAPE_REPRESENTATION('',(#6404),#10111);
#10263=SHAPE_REPRESENTATION('',(#6410,#6513,#6514,#6515,#6516,#6517,#6518),
#10112);
#10264=SHAPE_REPRESENTATION('',(#6411),#10113);
#10265=SHAPE_REPRESENTATION('',(#6427),#10114);
#10266=SHAPE_REPRESENTATION('',(#6462),#10115);
#10267=SHAPE_REPRESENTATION('',(#6473),#10116);
#10268=SHAPE_REPRESENTATION('',(#6482),#10117);
#10269=SHAPE_REPRESENTATION('',(#6489),#10118);
#10270=PRODUCT_DEFINITION_CONTEXT('part definition',#10362,'design');
#10271=PRODUCT_DEFINITION('PAT-043',
'PAT-043',#10301,#10270);
#10272=PRODUCT_DEFINITION('Header and valve bodies',
'Header and valve bodies',#10302,#10270);
#10273=PRODUCT_DEFINITION('Four-port header','Four-port header',#10303,
#10270);
#10274=PRODUCT_DEFINITION('Header end plug','Header end plug',#10304,#10270);
#10275=PRODUCT_DEFINITION('Header foot','Header foot',#10305,#10270);
#10276=PRODUCT_DEFINITION('Header foot (1)','Header foot (1)',#10306,#10270);
#10277=PRODUCT_DEFINITION('Hex Bolt - M6 x 30 mm',
'Hex Bolt - M6 x 30 mm',#10307,#10270);
#10278=PRODUCT_DEFINITION('Valve body','Valve body',#10308,#10270);
#10279=PRODUCT_DEFINITION('Body inlet half','Body inlet half',#10309,#10270);
#10280=PRODUCT_DEFINITION('Body outlet half','Body outlet half',#10310,
#10270);
#10281=PRODUCT_DEFINITION('Split-body gasket','Split-body gasket',#10311,
#10270);
#10282=PRODUCT_DEFINITION('Stem guide','Stem guide',#10312,#10270);
#10283=PRODUCT_DEFINITION('Packing ring','Packing ring',#10313,#10270);
#10284=PRODUCT_DEFINITION('Packing retainer','Packing retainer',#10314,
#10270);
#10285=PRODUCT_DEFINITION('Lever stop bridge','Lever stop bridge',#10315,
#10270);
#10286=PRODUCT_DEFINITION('Ball seat','Ball seat',#10316,#10270);
#10287=PRODUCT_DEFINITION('M5x70 body screw','M5x70 body screw',#10317,
#10270);
#10288=PRODUCT_DEFINITION('Flat Washer - M5','Flat Washer - M5',#10318,
#10270);
#10289=PRODUCT_DEFINITION('Hex Nut - M5','Hex Nut - M5',#10319,#10270);
#10290=PRODUCT_DEFINITION(
'Hex Pipe Nipple - 1-2 Inch Tapered Pipe Thread',
'Hex Pipe Nipple - 1-2 Inch Tapered Pipe Thread',#10320,#10270);
#10291=PRODUCT_DEFINITION('Bridge spacer','Bridge spacer',#10321,#10270);
#10292=PRODUCT_DEFINITION('Cap Screw - M4x16','Cap Screw - M4x16',#10322,
#10270);
#10293=PRODUCT_DEFINITION('Stop pin','Stop pin',#10323,#10270);
#10294=PRODUCT_DEFINITION('Valve rotor','Valve rotor',#10324,#10270);
#10295=PRODUCT_DEFINITION('Ported ball','Ported ball',#10325,#10270);
#10296=PRODUCT_DEFINITION('Stem','Stem',#10326,#10270);
#10297=PRODUCT_DEFINITION('Lever','Lever',#10327,#10270);
#10298=PRODUCT_DEFINITION('Lever keeper','Lever keeper',#10328,#10270);
#10299=PRODUCT_DEFINITION('Bonded grip','Bonded grip',#10329,#10270);
#10300=PRODUCT_DEFINITION('M4x10 Cap Screw','M4x10 Cap Screw',#10330,#10270);
#10301=PRODUCT_DEFINITION_FORMATION('',$,#10364);
#10302=PRODUCT_DEFINITION_FORMATION('',$,#10365);
#10303=PRODUCT_DEFINITION_FORMATION('',$,#10366);
#10304=PRODUCT_DEFINITION_FORMATION('',$,#10367);
#10305=PRODUCT_DEFINITION_FORMATION('',$,#10368);
#10306=PRODUCT_DEFINITION_FORMATION('',$,#10369);
#10307=PRODUCT_DEFINITION_FORMATION('',$,#10370);
#10308=PRODUCT_DEFINITION_FORMATION('',$,#10371);
#10309=PRODUCT_DEFINITION_FORMATION('',$,#10372);
#10310=PRODUCT_DEFINITION_FORMATION('',$,#10373);
#10311=PRODUCT_DEFINITION_FORMATION('',$,#10374);
#10312=PRODUCT_DEFINITION_FORMATION('',$,#10375);
#10313=PRODUCT_DEFINITION_FORMATION('',$,#10376);
#10314=PRODUCT_DEFINITION_FORMATION('',$,#10377);
#10315=PRODUCT_DEFINITION_FORMATION('',$,#10378);
#10316=PRODUCT_DEFINITION_FORMATION('',$,#10379);
#10317=PRODUCT_DEFINITION_FORMATION('',$,#10380);
#10318=PRODUCT_DEFINITION_FORMATION('',$,#10381);
#10319=PRODUCT_DEFINITION_FORMATION('',$,#10382);
#10320=PRODUCT_DEFINITION_FORMATION('',$,#10383);
#10321=PRODUCT_DEFINITION_FORMATION('',$,#10384);
#10322=PRODUCT_DEFINITION_FORMATION('',$,#10385);
#10323=PRODUCT_DEFINITION_FORMATION('',$,#10386);
#10324=PRODUCT_DEFINITION_FORMATION('',$,#10387);
#10325=PRODUCT_DEFINITION_FORMATION('',$,#10388);
#10326=PRODUCT_DEFINITION_FORMATION('',$,#10389);
#10327=PRODUCT_DEFINITION_FORMATION('',$,#10390);
#10328=PRODUCT_DEFINITION_FORMATION('',$,#10391);
#10329=PRODUCT_DEFINITION_FORMATION('',$,#10392);
#10330=PRODUCT_DEFINITION_FORMATION('',$,#10393);
#10331=PRODUCT_RELATED_PRODUCT_CATEGORY('PAT-043',
'PAT-043',(#10364));
#10332=PRODUCT_RELATED_PRODUCT_CATEGORY('Header and valve bodies',
'Header and valve bodies',(#10365));
#10333=PRODUCT_RELATED_PRODUCT_CATEGORY('Four-port header',
'Four-port header',(#10366));
#10334=PRODUCT_RELATED_PRODUCT_CATEGORY('Header end plug',
'Header end plug',(#10367));
#10335=PRODUCT_RELATED_PRODUCT_CATEGORY('Header foot','Header foot',(#10368));
#10336=PRODUCT_RELATED_PRODUCT_CATEGORY('Header foot (1)',
'Header foot (1)',(#10369));
#10337=PRODUCT_RELATED_PRODUCT_CATEGORY('Hex Bolt - M6 x 30 mm',
'Hex Bolt - M6 x 30 mm',(#10370));
#10338=PRODUCT_RELATED_PRODUCT_CATEGORY('Valve body','Valve body',(#10371));
#10339=PRODUCT_RELATED_PRODUCT_CATEGORY('Body inlet half',
'Body inlet half',(#10372));
#10340=PRODUCT_RELATED_PRODUCT_CATEGORY('Body outlet half',
'Body outlet half',(#10373));
#10341=PRODUCT_RELATED_PRODUCT_CATEGORY('Split-body gasket',
'Split-body gasket',(#10374));
#10342=PRODUCT_RELATED_PRODUCT_CATEGORY('Stem guide','Stem guide',(#10375));
#10343=PRODUCT_RELATED_PRODUCT_CATEGORY('Packing ring','Packing ring',(#10376));
#10344=PRODUCT_RELATED_PRODUCT_CATEGORY('Packing retainer',
'Packing retainer',(#10377));
#10345=PRODUCT_RELATED_PRODUCT_CATEGORY('Lever stop bridge',
'Lever stop bridge',(#10378));
#10346=PRODUCT_RELATED_PRODUCT_CATEGORY('Ball seat','Ball seat',(#10379));
#10347=PRODUCT_RELATED_PRODUCT_CATEGORY('M5x70 body screw',
'M5x70 body screw',(#10380));
#10348=PRODUCT_RELATED_PRODUCT_CATEGORY('Flat Washer - M5',
'Flat Washer - M5',(#10381));
#10349=PRODUCT_RELATED_PRODUCT_CATEGORY('Hex Nut - M5','Hex Nut - M5',(#10382));
#10350=PRODUCT_RELATED_PRODUCT_CATEGORY(
'Hex Pipe Nipple - 1-2 Inch Tapered Pipe Thread',
'Hex Pipe Nipple - 1-2 Inch Tapered Pipe Thread',(#10383));
#10351=PRODUCT_RELATED_PRODUCT_CATEGORY('Bridge spacer','Bridge spacer',
(#10384));
#10352=PRODUCT_RELATED_PRODUCT_CATEGORY('Cap Screw - M4x16',
'Cap Screw - M4x16',(#10385));
#10353=PRODUCT_RELATED_PRODUCT_CATEGORY('Stop pin','Stop pin',(#10386));
#10354=PRODUCT_RELATED_PRODUCT_CATEGORY('Valve rotor','Valve rotor',(#10387));
#10355=PRODUCT_RELATED_PRODUCT_CATEGORY('Ported ball','Ported ball',(#10388));
#10356=PRODUCT_RELATED_PRODUCT_CATEGORY('Stem','Stem',(#10389));
#10357=PRODUCT_RELATED_PRODUCT_CATEGORY('Lever','Lever',(#10390));
#10358=PRODUCT_RELATED_PRODUCT_CATEGORY('Lever keeper','Lever keeper',(#10391));
#10359=PRODUCT_RELATED_PRODUCT_CATEGORY('Bonded grip','Bonded grip',(#10392));
#10360=PRODUCT_RELATED_PRODUCT_CATEGORY('M4x10 Cap Screw',
'M4x10 Cap Screw',(#10393));
#10361=APPLICATION_PROTOCOL_DEFINITION('international standard',
'automotive_design',2009,#10362);
#10362=APPLICATION_CONTEXT(
'Core Data for Automotive Mechanical Design Process');
#10363=PRODUCT_CONTEXT('part definition',#10362,'mechanical');
#10364=PRODUCT('PAT-043','PAT-043',
'PAT-043',(#10363));
#10365=PRODUCT('Header and valve bodies','Header and valve bodies',
'Header and valve bodies',(#10363));
#10366=PRODUCT('Four-port header','Four-port header','Four-port header',
(#10363));
#10367=PRODUCT('Header end plug','Header end plug','Header end plug',(#10363));
#10368=PRODUCT('Header foot','Header foot','Header foot',(#10363));
#10369=PRODUCT('Header foot (1)','Header foot (1)','Header foot (1)',(#10363));
#10370=PRODUCT('Hex Bolt - M6 x 30 mm','Hex Bolt - M6 x 30 mm',
'Hex Bolt - M6 x 30 mm',(#10363));
#10371=PRODUCT('Valve body','Valve body','Valve body',(#10363));
#10372=PRODUCT('Body inlet half','Body inlet half','Body inlet half',(#10363));
#10373=PRODUCT('Body outlet half','Body outlet half','Body outlet half',
(#10363));
#10374=PRODUCT('Split-body gasket','Split-body gasket',
'Split-body gasket',(#10363));
#10375=PRODUCT('Stem guide','Stem guide','Stem guide',(#10363));
#10376=PRODUCT('Packing ring','Packing ring','Packing ring',(#10363));
#10377=PRODUCT('Packing retainer','Packing retainer','Packing retainer',
(#10363));
#10378=PRODUCT('Lever stop bridge','Lever stop bridge',
'Lever stop bridge',(#10363));
#10379=PRODUCT('Ball seat','Ball seat','Ball seat',(#10363));
#10380=PRODUCT('M5x70 body screw','M5x70 body screw','M5x70 body screw',
(#10363));
#10381=PRODUCT('Flat Washer - M5','Flat Washer - M5','Flat Washer - M5',
(#10363));
#10382=PRODUCT('Hex Nut - M5','Hex Nut - M5','Hex Nut - M5',(#10363));
#10383=PRODUCT('Hex Pipe Nipple - 1-2 Inch Tapered Pipe Thread',
'Hex Pipe Nipple - 1-2 Inch Tapered Pipe Thread',
'Hex Pipe Nipple - 1-2 Inch Tapered Pipe Thread',(#10363));
#10384=PRODUCT('Bridge spacer','Bridge spacer','Bridge spacer',(#10363));
#10385=PRODUCT('Cap Screw - M4x16','Cap Screw - M4x16',
'Cap Screw - M4x16',(#10363));
#10386=PRODUCT('Stop pin','Stop pin','Stop pin',(#10363));
#10387=PRODUCT('Valve rotor','Valve rotor',
'Valve rotor',(#10363));
#10388=PRODUCT('Ported ball','Ported ball','Ported ball',(#10363));
#10389=PRODUCT('Stem','Stem','Stem',(#10363));
#10390=PRODUCT('Lever','Lever',
'Lever',(#10363));
#10391=PRODUCT('Lever keeper','Lever keeper','Lever keeper',(#10363));
#10392=PRODUCT('Bonded grip','Bonded grip','Bonded grip',(#10363));
#10393=PRODUCT('M4x10 Cap Screw','M4x10 Cap Screw','M4x10 Cap Screw',(#10363));
#10394=PRESENTATION_STYLE_ASSIGNMENT((#10401));
#10395=PRESENTATION_STYLE_ASSIGNMENT((#10402));
#10396=PRESENTATION_STYLE_ASSIGNMENT((#10403));
#10397=PRESENTATION_STYLE_ASSIGNMENT((#10404));
#10398=PRESENTATION_STYLE_ASSIGNMENT((#10405));
#10399=PRESENTATION_STYLE_ASSIGNMENT((#10406));
#10400=PRESENTATION_STYLE_ASSIGNMENT((#10407));
#10401=SURFACE_STYLE_USAGE(.BOTH.,#10408);
#10402=SURFACE_STYLE_USAGE(.BOTH.,#10409);
#10403=SURFACE_STYLE_USAGE(.BOTH.,#10410);
#10404=SURFACE_STYLE_USAGE(.BOTH.,#10411);
#10405=SURFACE_STYLE_USAGE(.BOTH.,#10412);
#10406=SURFACE_STYLE_USAGE(.BOTH.,#10413);
#10407=SURFACE_STYLE_USAGE(.BOTH.,#10414);
#10408=SURFACE_SIDE_STYLE('',(#10415));
#10409=SURFACE_SIDE_STYLE('',(#10416));
#10410=SURFACE_SIDE_STYLE('',(#10417));
#10411=SURFACE_SIDE_STYLE('',(#10418));
#10412=SURFACE_SIDE_STYLE('',(#10419));
#10413=SURFACE_SIDE_STYLE('',(#10420));
#10414=SURFACE_SIDE_STYLE('',(#10421));
#10415=SURFACE_STYLE_FILL_AREA(#10422);
#10416=SURFACE_STYLE_FILL_AREA(#10423);
#10417=SURFACE_STYLE_FILL_AREA(#10424);
#10418=SURFACE_STYLE_FILL_AREA(#10425);
#10419=SURFACE_STYLE_FILL_AREA(#10426);
#10420=SURFACE_STYLE_FILL_AREA(#10427);
#10421=SURFACE_STYLE_FILL_AREA(#10428);
#10422=FILL_AREA_STYLE('Steel - Satin',(#10429));
#10423=FILL_AREA_STYLE('CAD Library Painted - Engineering blue',(#10430));
#10424=FILL_AREA_STYLE('CAD Library Painted - Off white',(#10431));
#10425=FILL_AREA_STYLE('CAD Library Painted - Deep blue',(#10432));
#10426=FILL_AREA_STYLE('CAD Library Painted - Graphite',(#10433));
#10427=FILL_AREA_STYLE('CAD Library Painted - Steel gray',(#10434));
#10428=FILL_AREA_STYLE('CAD Library Painted - Light blue',(#10435));
#10429=FILL_AREA_STYLE_COLOUR('Steel - Satin',#10436);
#10430=FILL_AREA_STYLE_COLOUR('CAD Library Painted - Engineering blue',
#10437);
#10431=FILL_AREA_STYLE_COLOUR('CAD Library Painted - Off white',#10438);
#10432=FILL_AREA_STYLE_COLOUR('CAD Library Painted - Deep blue',#10439);
#10433=FILL_AREA_STYLE_COLOUR('CAD Library Painted - Graphite',#10440);
#10434=FILL_AREA_STYLE_COLOUR('CAD Library Painted - Steel gray',#10441);
#10435=FILL_AREA_STYLE_COLOUR('CAD Library Painted - Light blue',#10442);
#10436=COLOUR_RGB('Steel - Satin',0.627450980392157,0.627450980392157,0.627450980392157);
#10437=COLOUR_RGB('CAD Library Painted - Engineering blue',0.12156862745098,
0.356862745098039,0.6);
#10438=COLOUR_RGB('CAD Library Painted - Off white',0.909803921568627,0.901960784313726,
0.858823529411765);
#10439=COLOUR_RGB('CAD Library Painted - Deep blue',0.0784313725490196,
0.203921568627451,0.349019607843137);
#10440=COLOUR_RGB('CAD Library Painted - Graphite',0.0980392156862745,0.109803921568627,
0.125490196078431);
#10441=COLOUR_RGB('CAD Library Painted - Steel gray',0.592156862745098,
0.631372549019608,0.67843137254902);
#10442=COLOUR_RGB('CAD Library Painted - Light blue',0.286274509803922,
0.552941176470588,0.780392156862745);
#10443=COLOUR_RGB('Dark Blue',0.08,0.2,0.34);
#10444=FILL_AREA_STYLE_COLOUR('',#10443);
#10445=FILL_AREA_STYLE('',(#10444));
#10446=SURFACE_STYLE_FILL_AREA(#10445);
#10447=SURFACE_SIDE_STYLE('',(#10446));
#10448=SURFACE_STYLE_USAGE(.BOTH.,#10447);
#10449=PRESENTATION_STYLE_ASSIGNMENT((#10448));
#10450=COLOUR_RGB('Light Blue',0.38,0.62,0.78);
#10451=FILL_AREA_STYLE_COLOUR('',#10450);
#10452=FILL_AREA_STYLE('',(#10451));
#10453=SURFACE_STYLE_FILL_AREA(#10452);
#10454=SURFACE_SIDE_STYLE('',(#10453));
#10455=SURFACE_STYLE_USAGE(.BOTH.,#10454);
#10456=PRESENTATION_STYLE_ASSIGNMENT((#10455));
#10457=COLOUR_RGB('Sky Blue',0.24,0.69,0.87);
#10458=FILL_AREA_STYLE_COLOUR('',#10457);
#10459=FILL_AREA_STYLE('',(#10458));
#10460=SURFACE_STYLE_FILL_AREA(#10459);
#10461=SURFACE_SIDE_STYLE('',(#10460));
#10462=SURFACE_STYLE_USAGE(.BOTH.,#10461);
#10463=PRESENTATION_STYLE_ASSIGNMENT((#10462));
#10464=COLOUR_RGB('Grey',0.48,0.52,0.57);
#10465=FILL_AREA_STYLE_COLOUR('',#10464);
#10466=FILL_AREA_STYLE('',(#10465));
#10467=SURFACE_STYLE_FILL_AREA(#10466);
#10468=SURFACE_SIDE_STYLE('',(#10467));
#10469=SURFACE_STYLE_USAGE(.BOTH.,#10468);
#10470=PRESENTATION_STYLE_ASSIGNMENT((#10469));
#10471=COLOUR_RGB('Black',0.12,0.14,0.17);
#10472=FILL_AREA_STYLE_COLOUR('',#10471);
#10473=FILL_AREA_STYLE('',(#10472));
#10474=SURFACE_STYLE_FILL_AREA(#10473);
#10475=SURFACE_SIDE_STYLE('',(#10474));
#10476=SURFACE_STYLE_USAGE(.BOTH.,#10475);
#10477=PRESENTATION_STYLE_ASSIGNMENT((#10476));
#10478=COLOUR_RGB('Off White',0.89,0.88,0.83);
#10479=FILL_AREA_STYLE_COLOUR('',#10478);
#10480=FILL_AREA_STYLE('',(#10479));
#10481=SURFACE_STYLE_FILL_AREA(#10480);
#10482=SURFACE_SIDE_STYLE('',(#10481));
#10483=SURFACE_STYLE_USAGE(.BOTH.,#10482);
#10484=PRESENTATION_STYLE_ASSIGNMENT((#10483));
ENDSEC;
END-ISO-10303-21;
